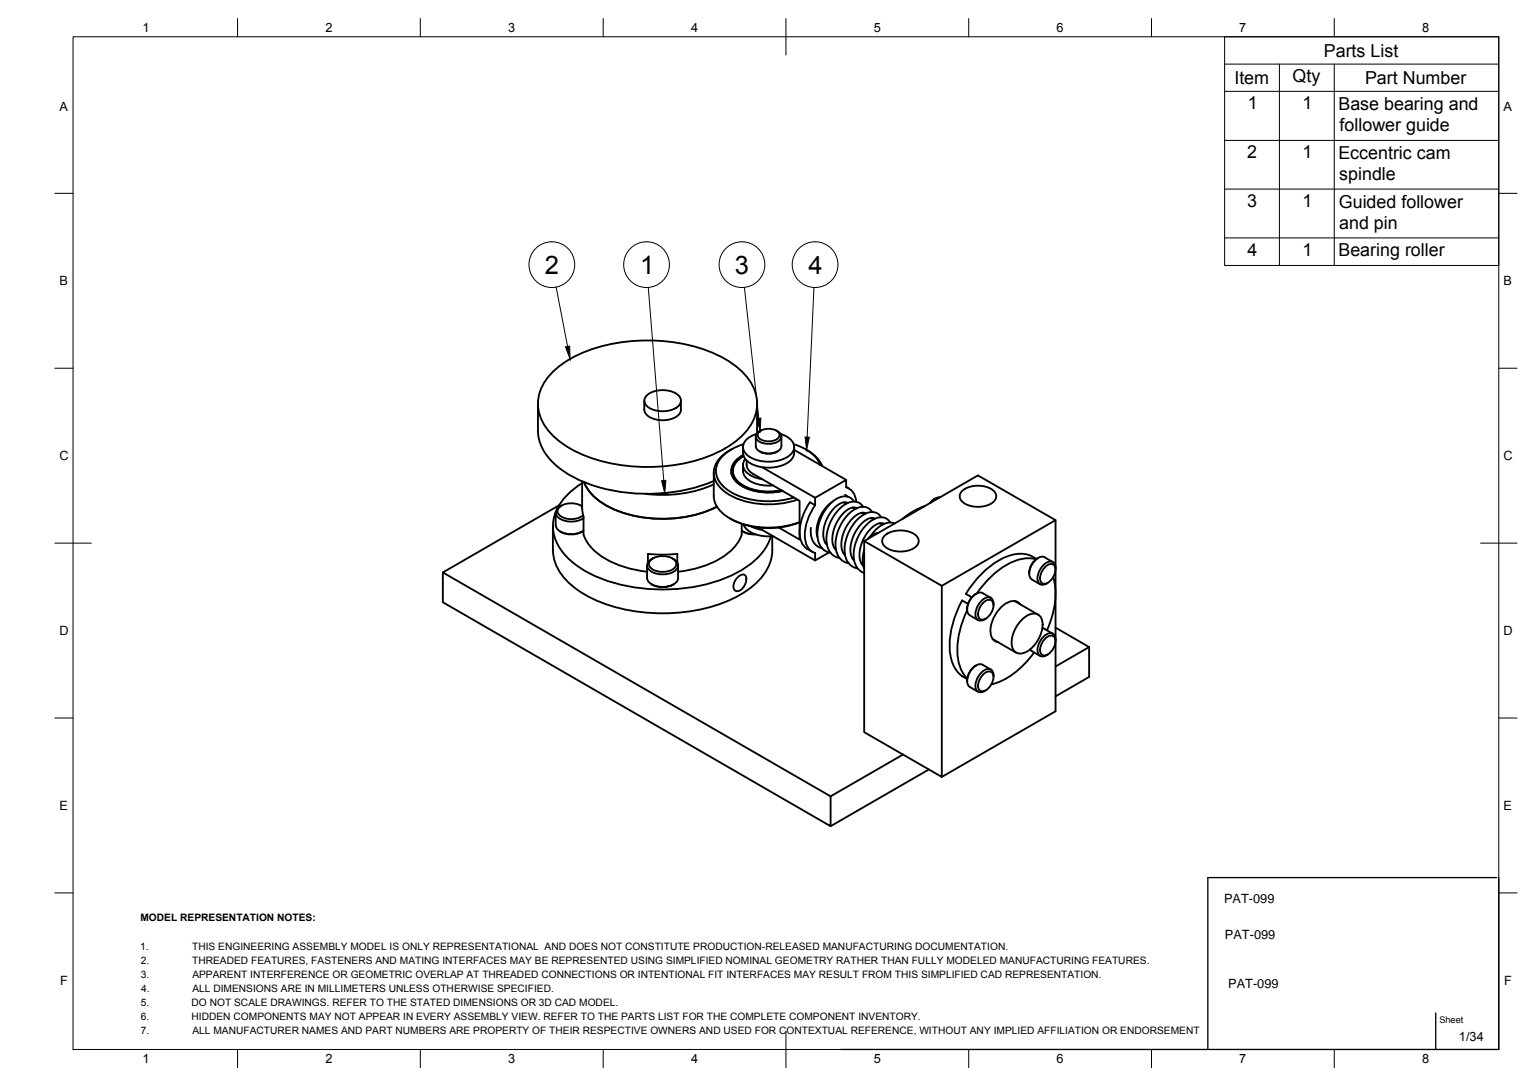
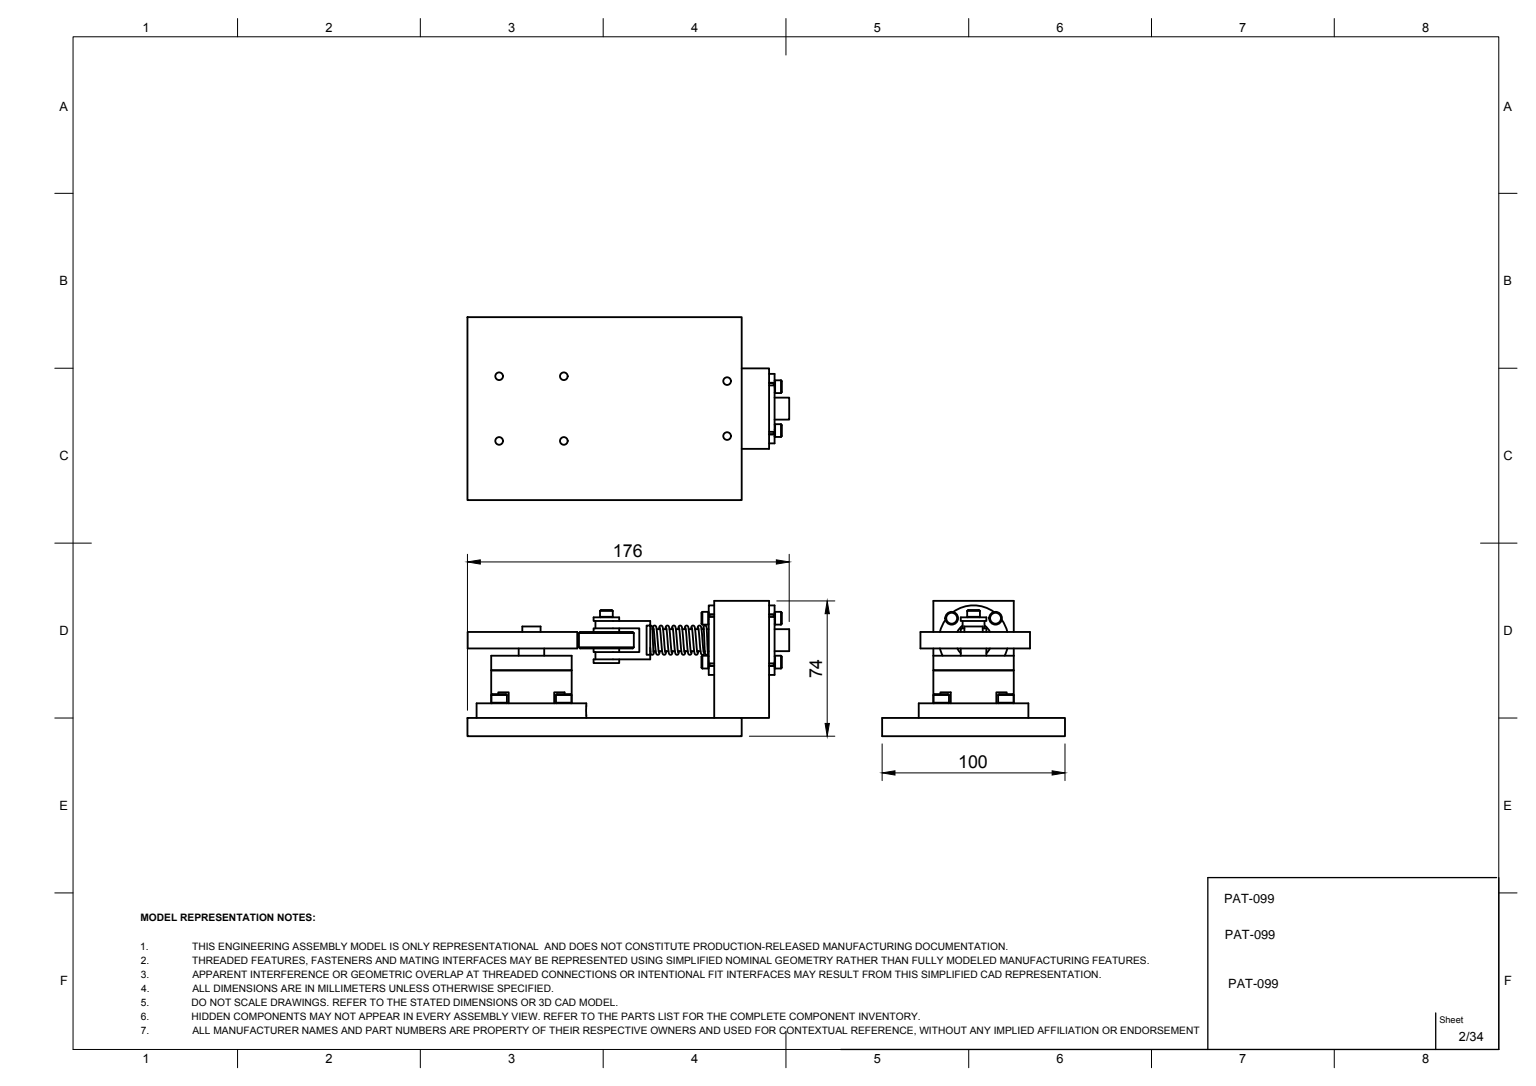
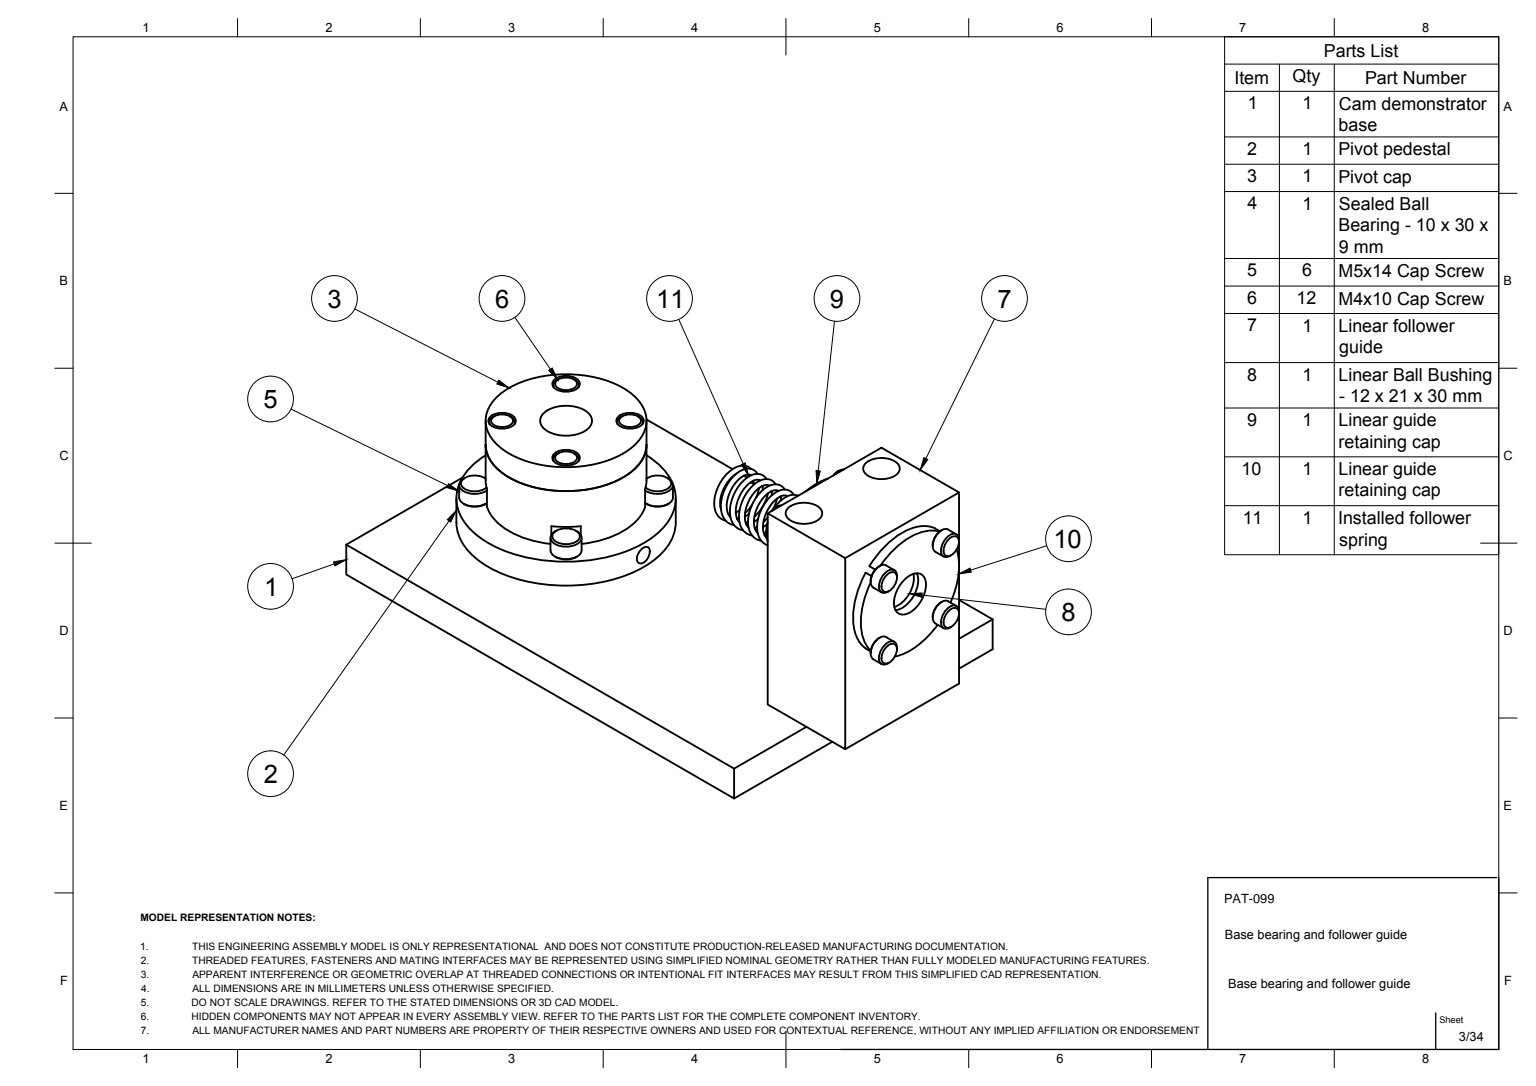
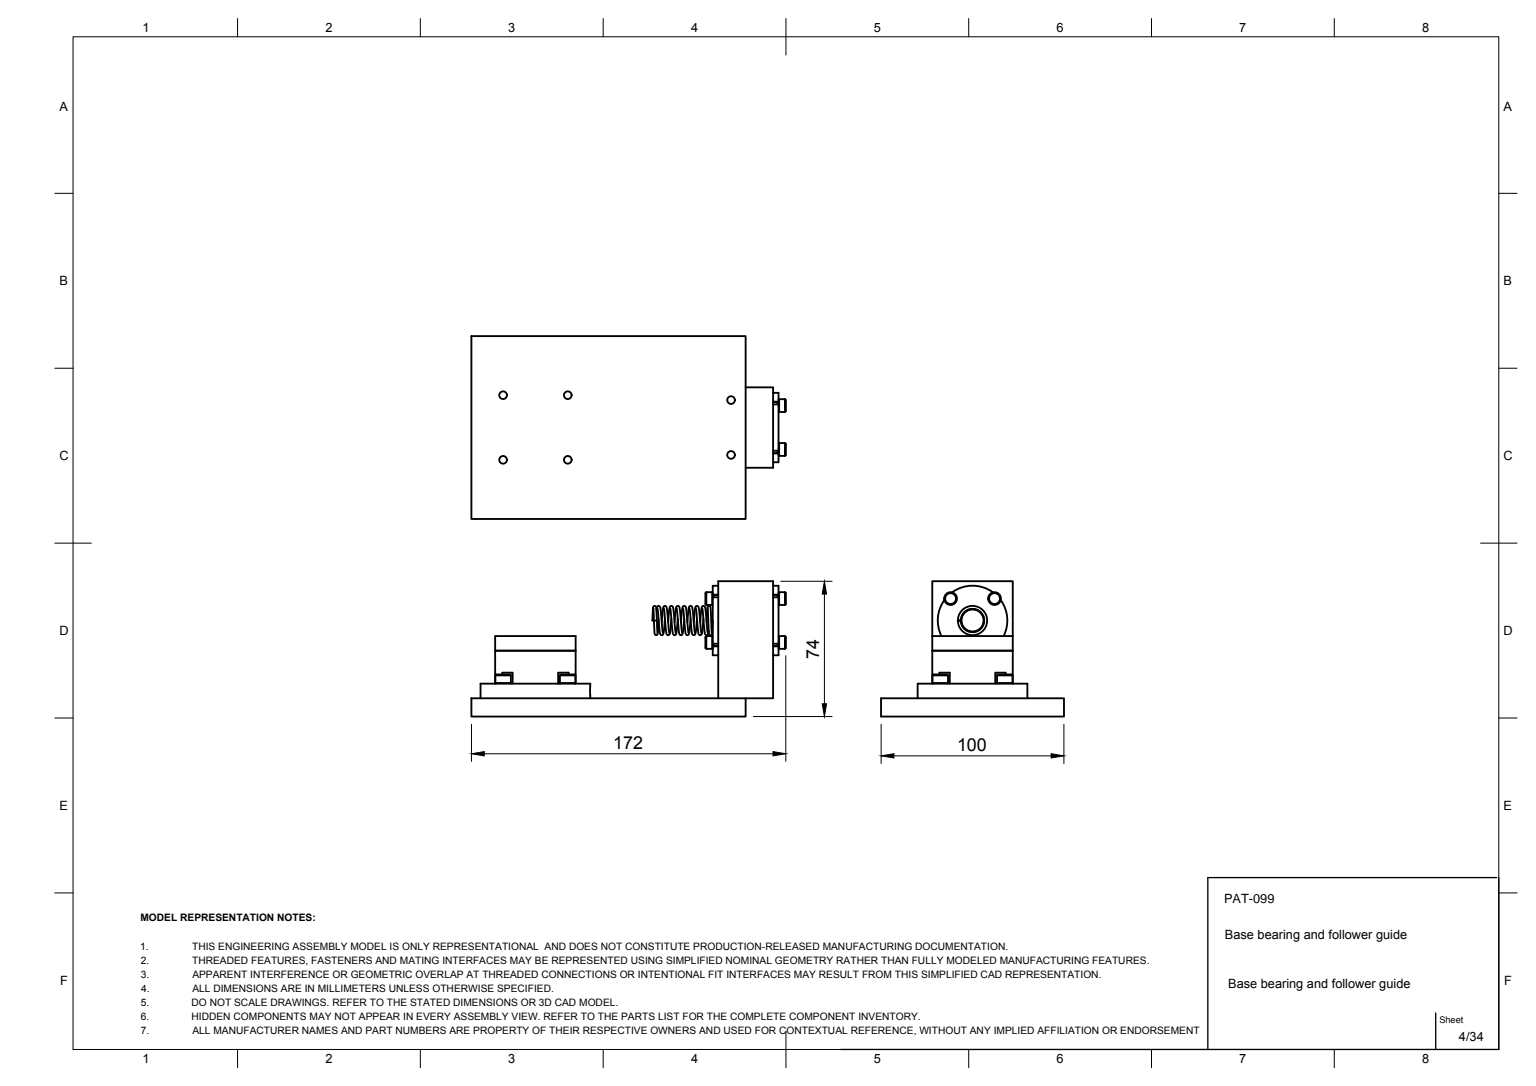
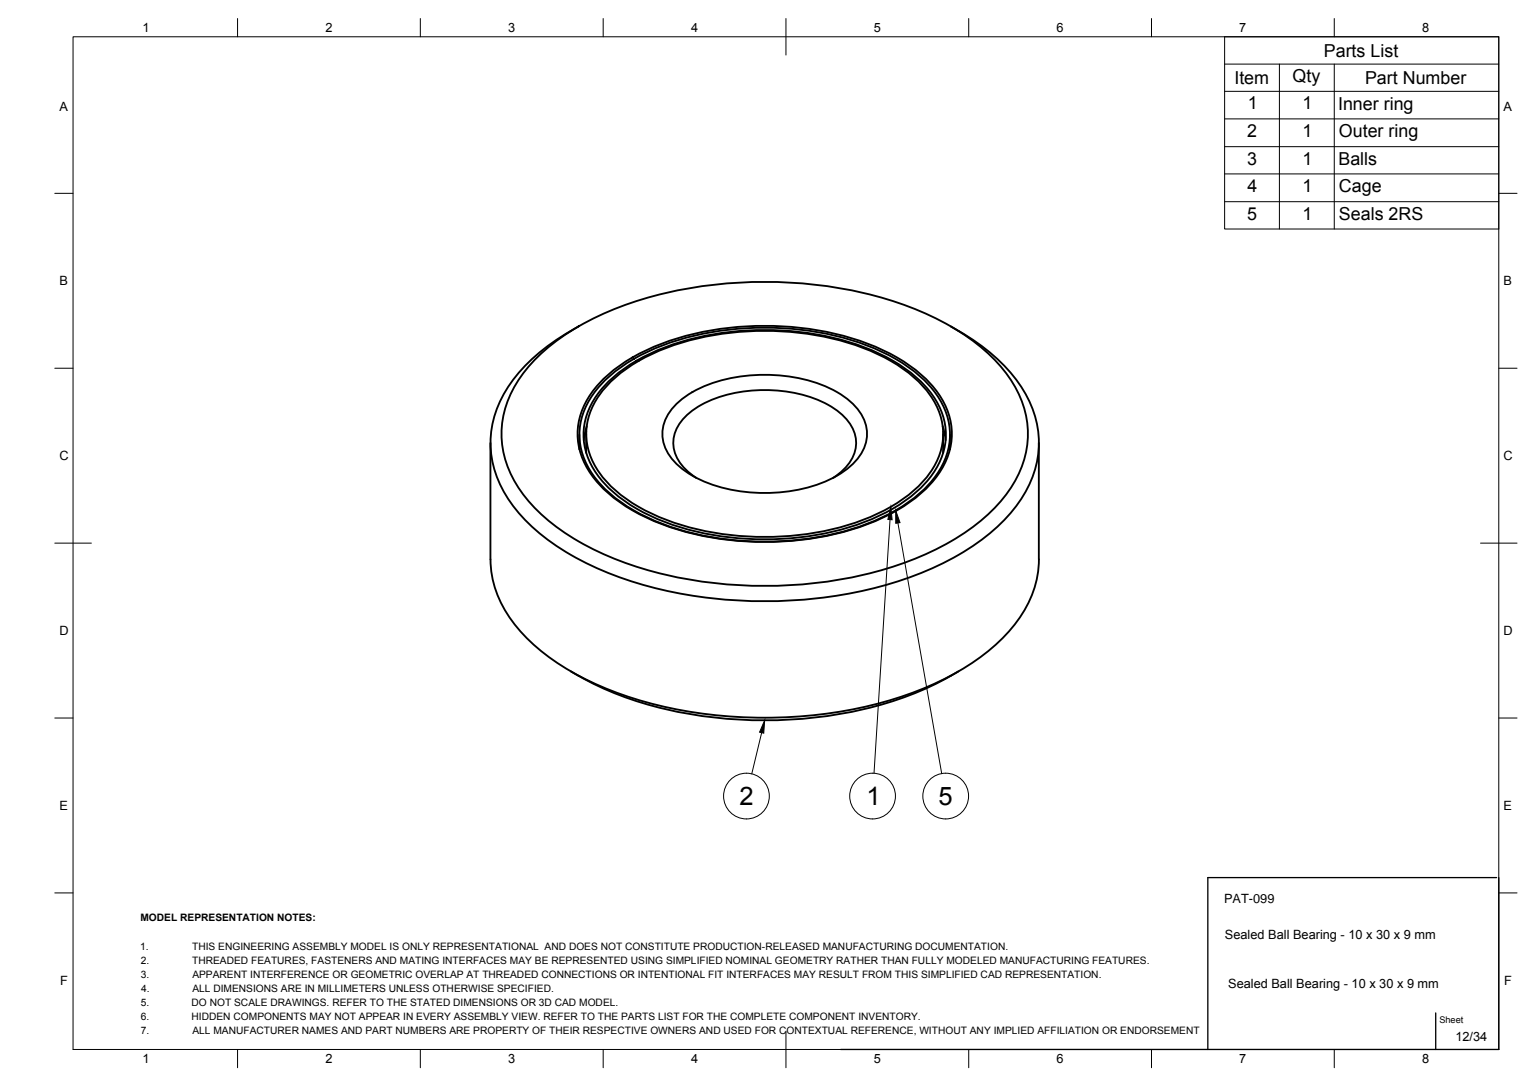
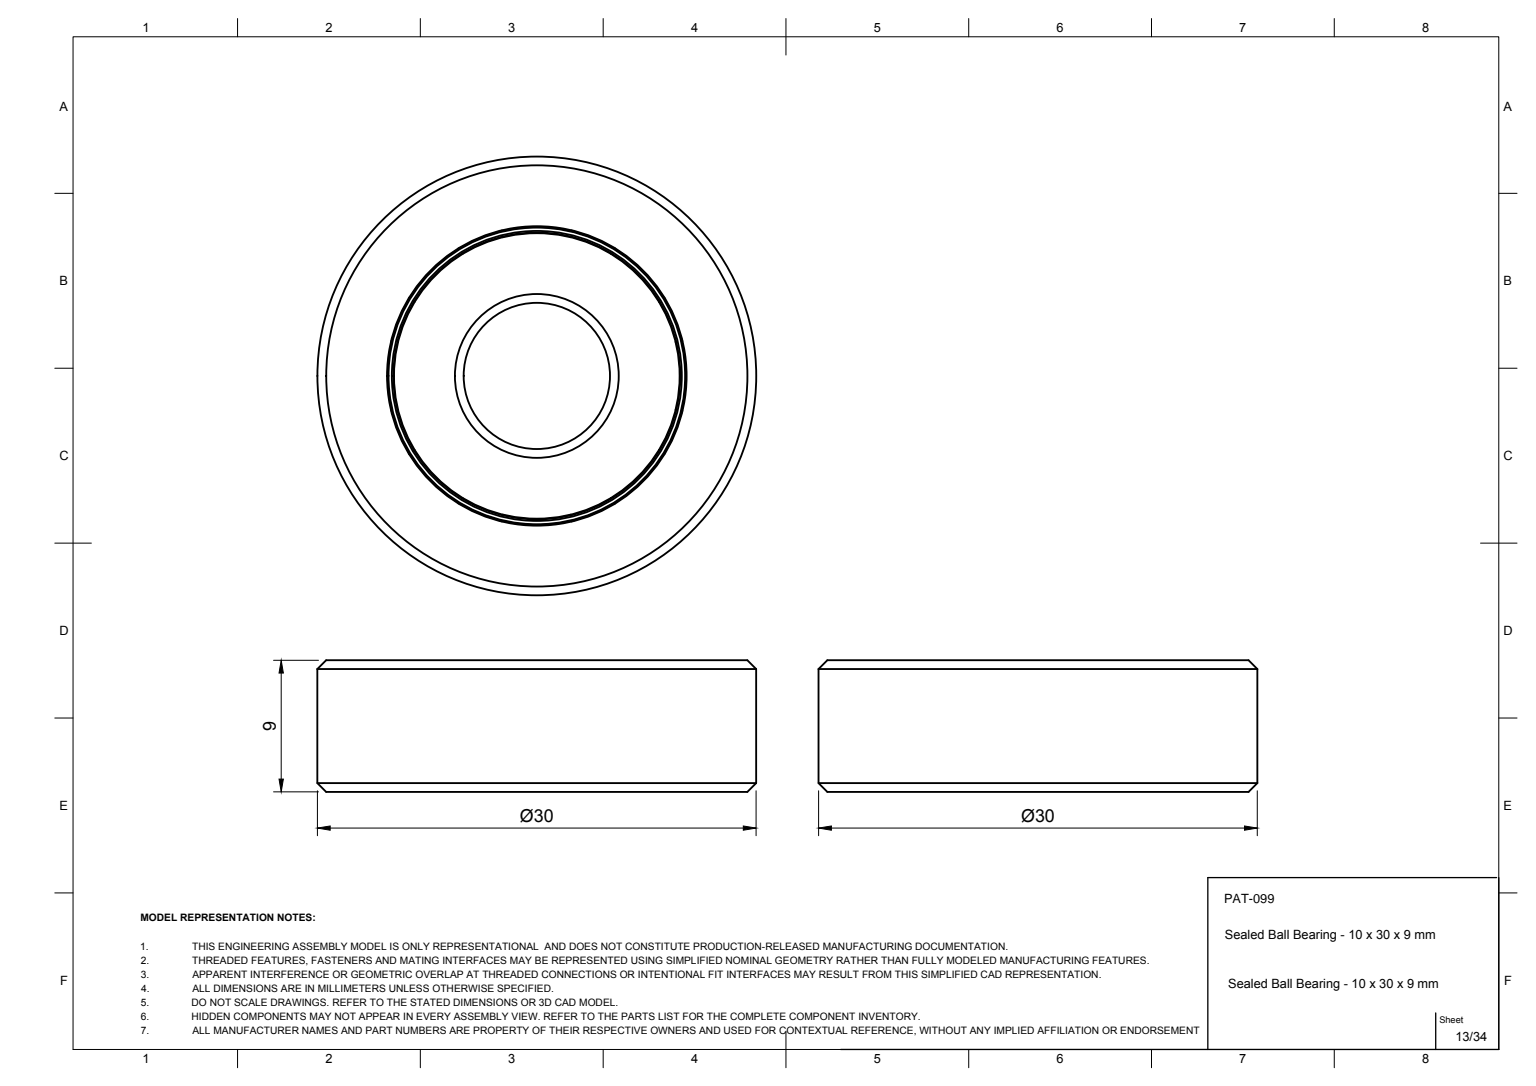
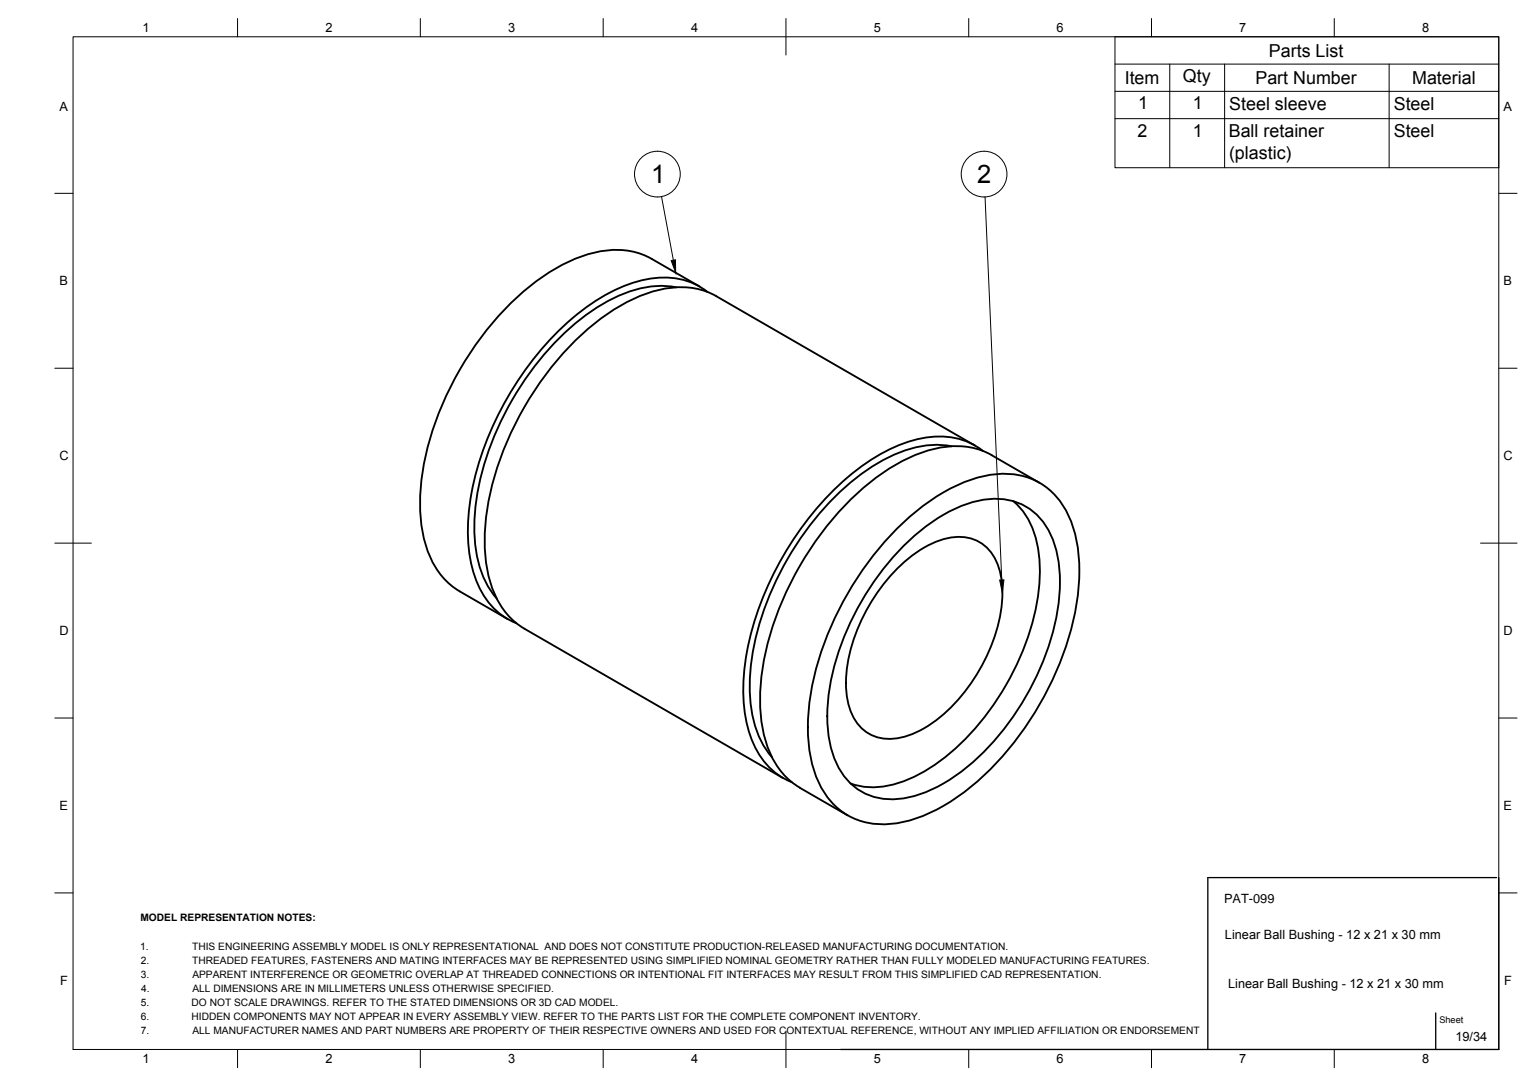
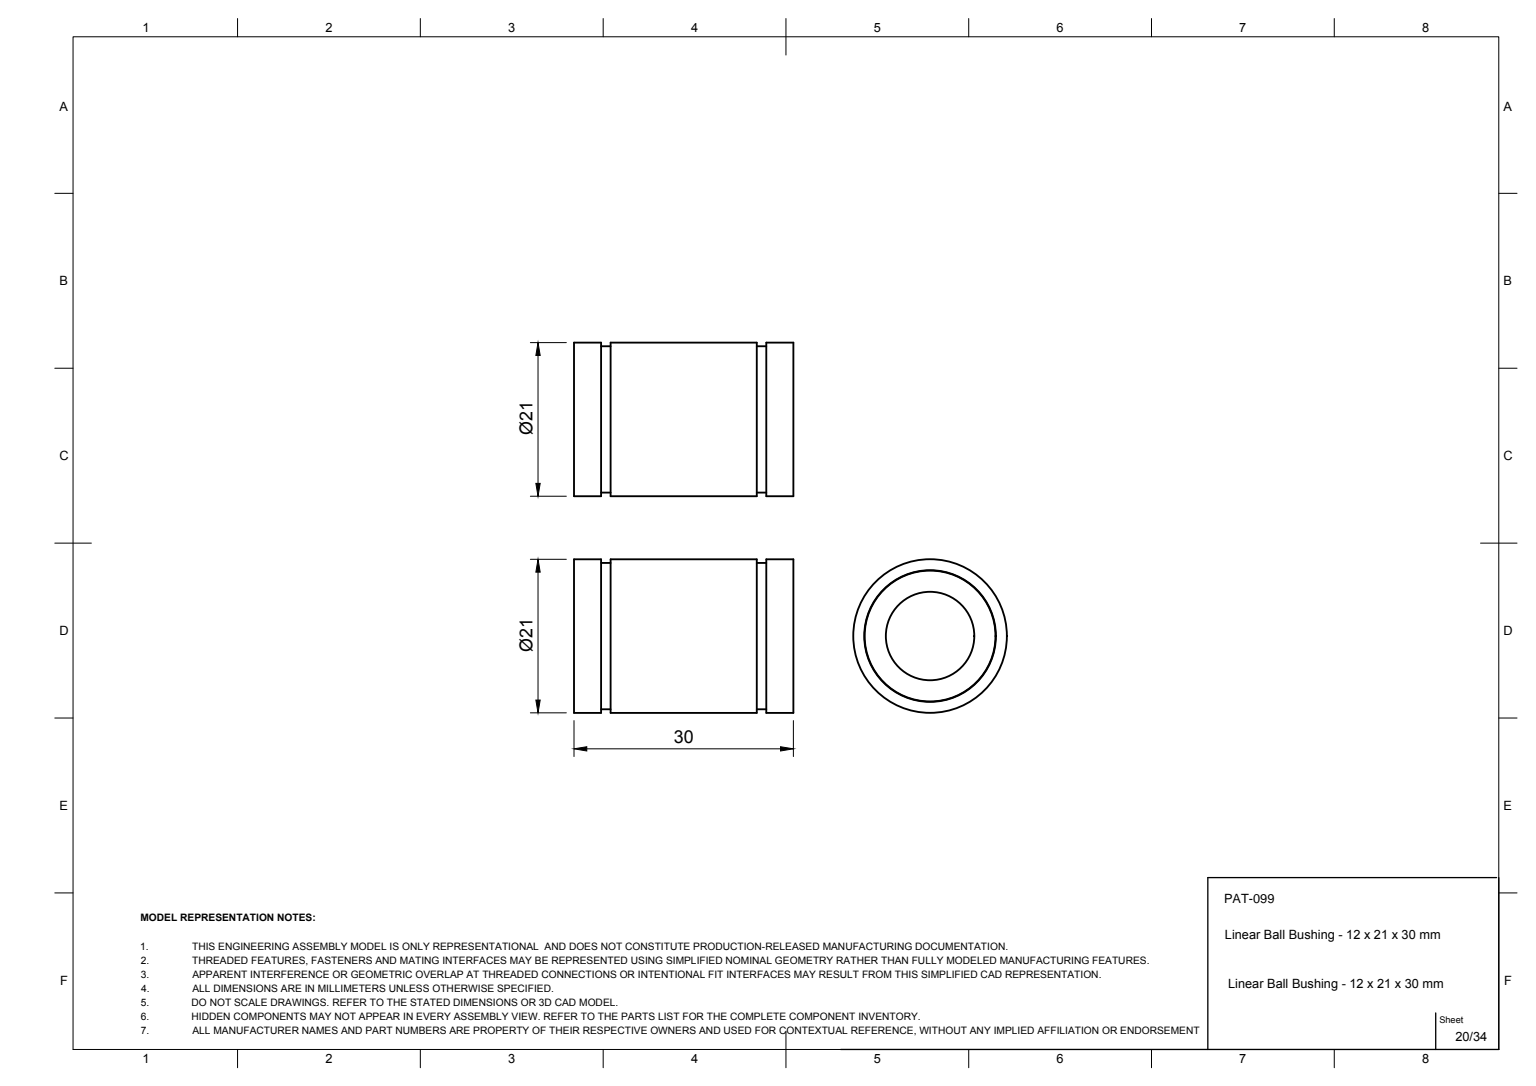
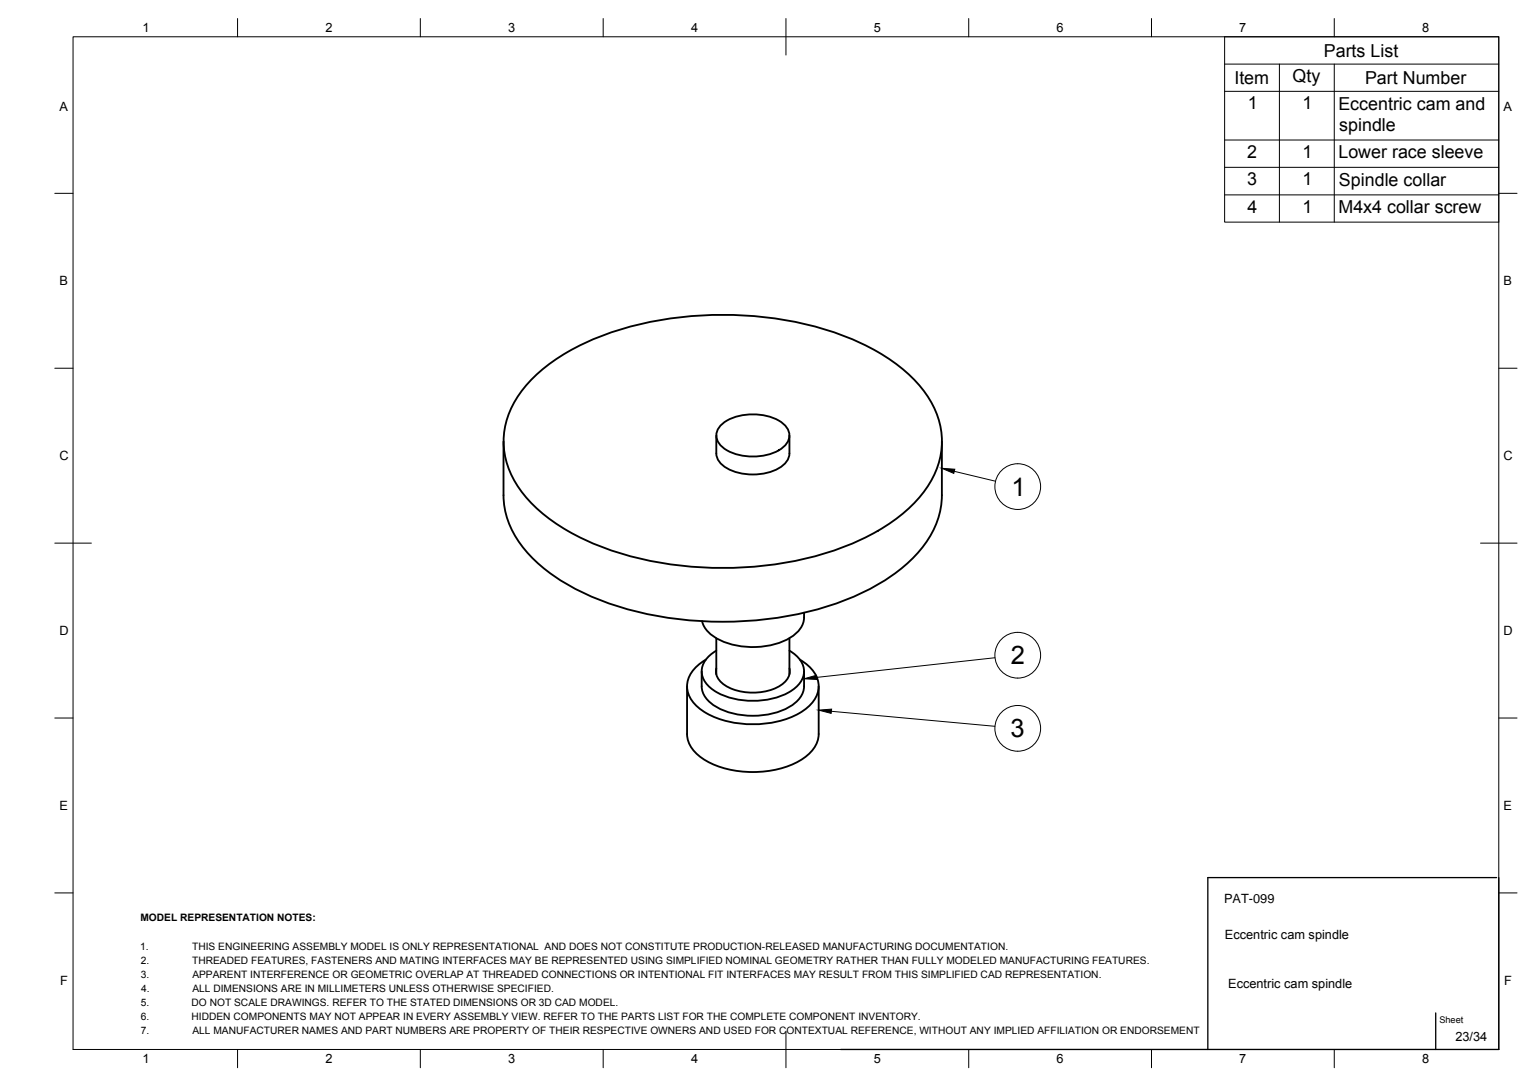
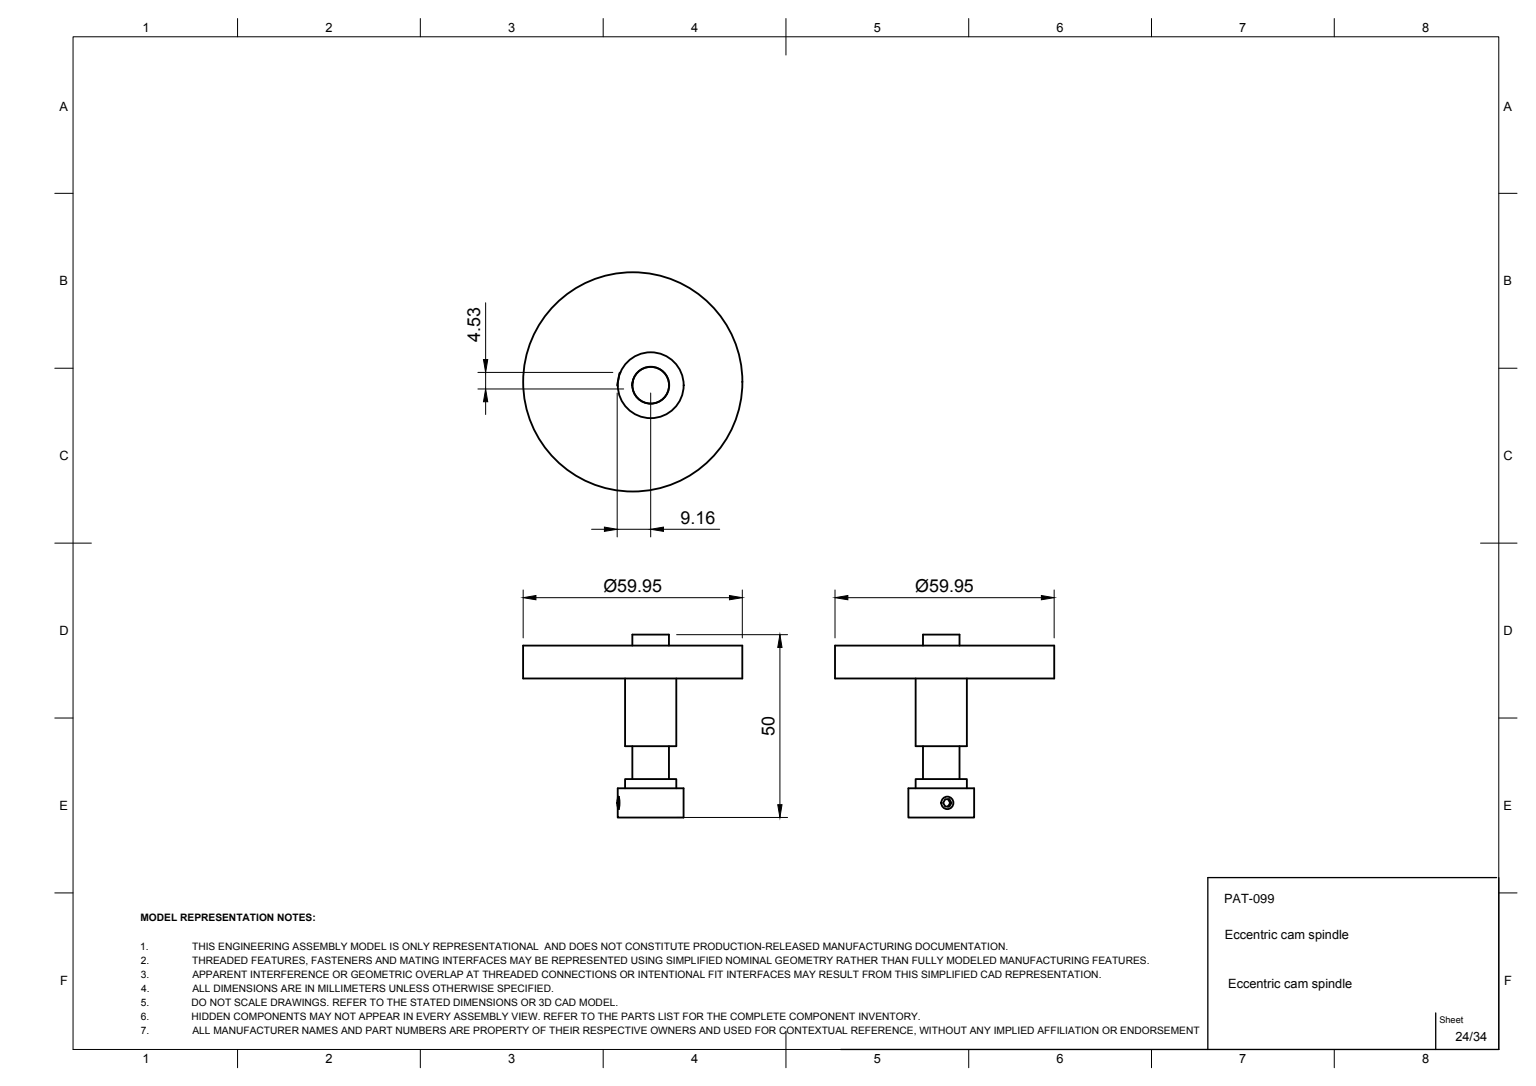
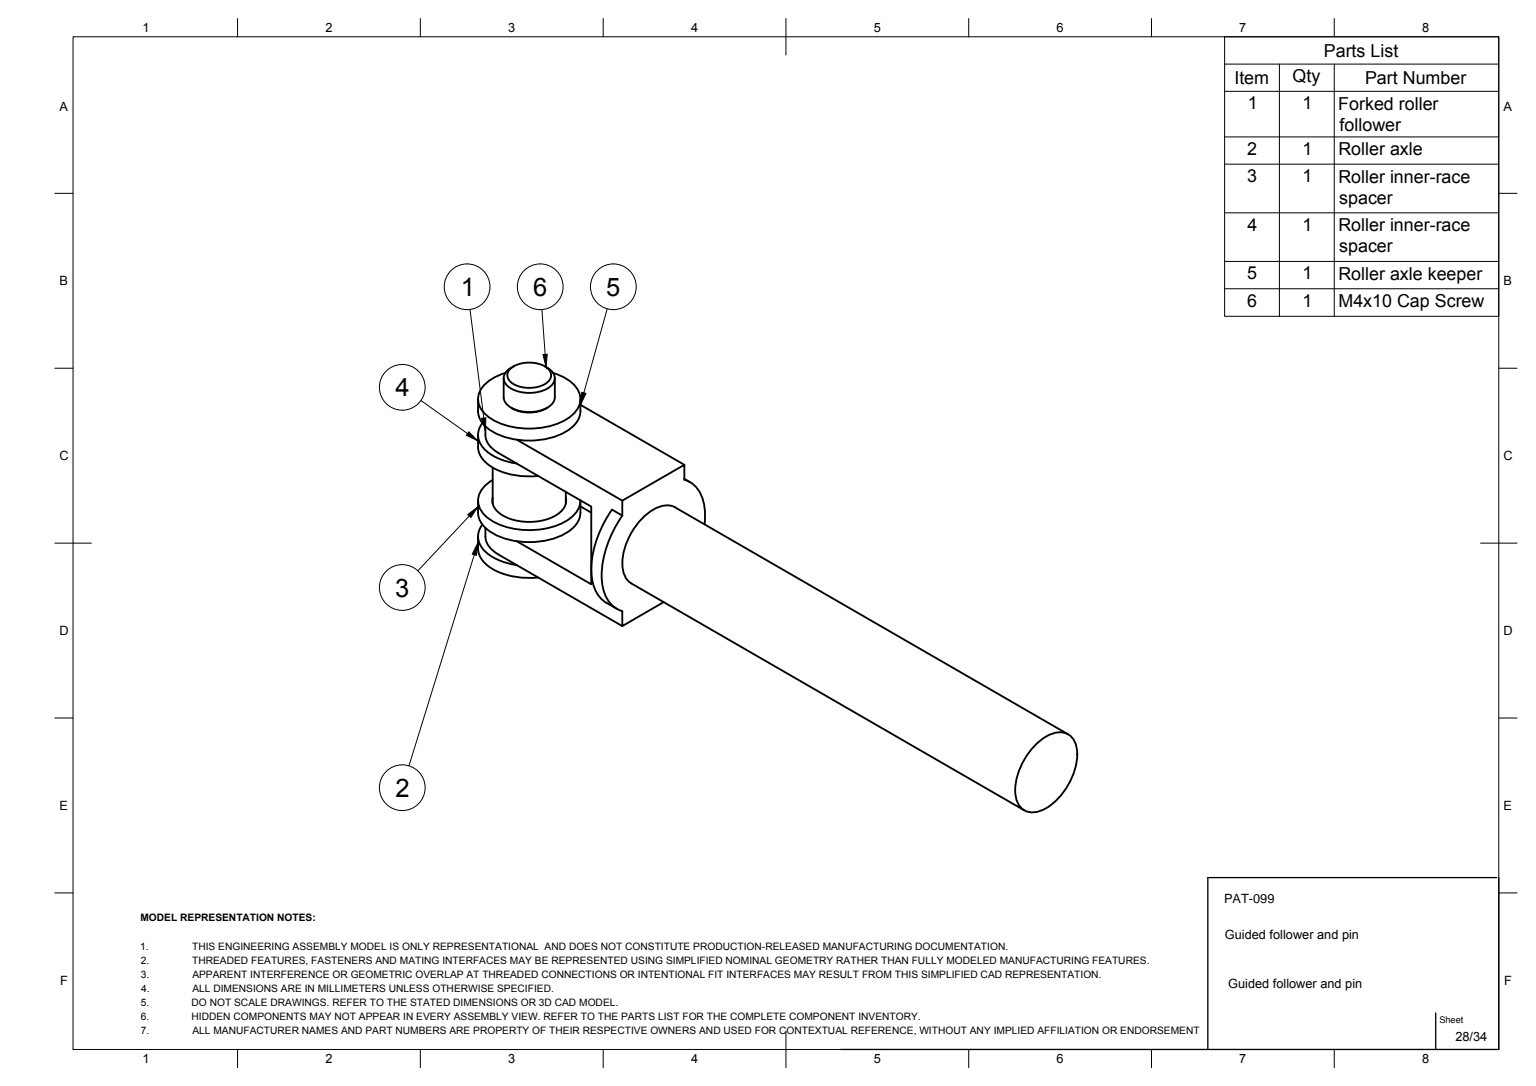
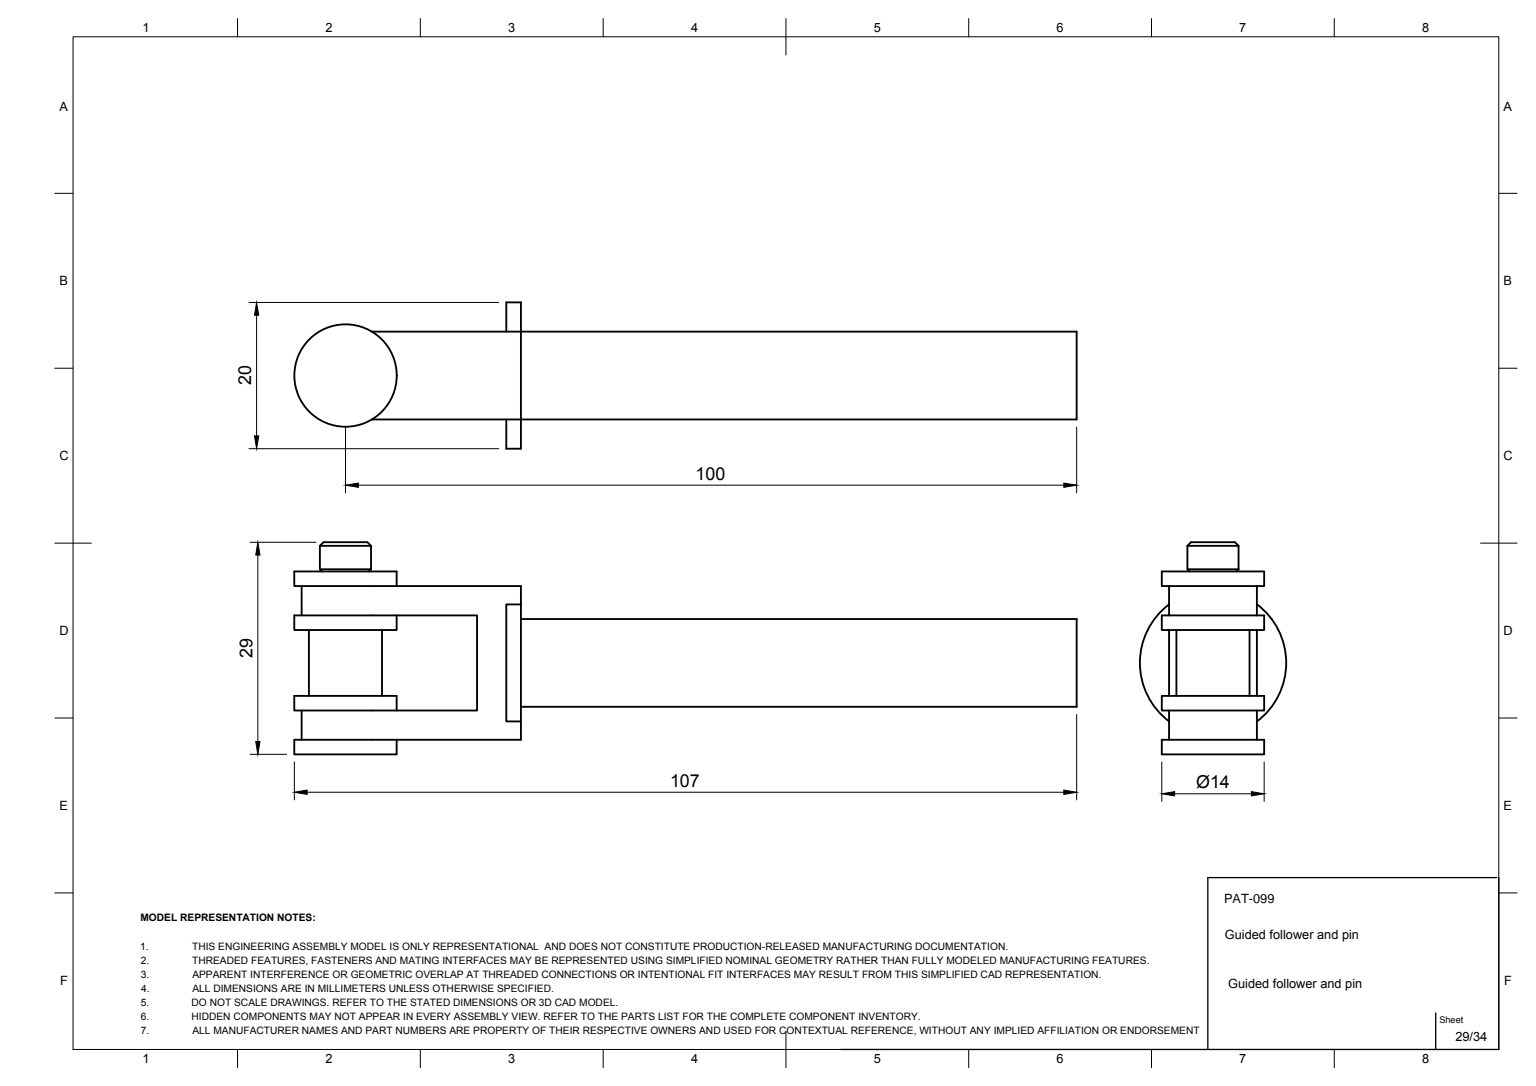
ISO-10303-21;
HEADER;
/* Generated by software containing ST-Developer
 * from STEP Tools, Inc. (www.steptools.com) 
 */

FILE_DESCRIPTION(
/* description */ ('PAT-099'),
/* implementation_level */ '2;1');

FILE_NAME(
/* name */ 'PAT-099',
/* time_stamp */ '2026-10-29T17:25:42-07:00',
/* author */ (''),
/* organization */ (''),
/* preprocessor_version */ 'ST-DEVELOPER v20.2',
/* originating_system */ 'Autodesk Translation Framework v15.17.0.0',
/* authorisation */ '');

FILE_SCHEMA (('AUTOMOTIVE_DESIGN { 1 0 10303 214 3 1 1 }'));
ENDSEC;

DATA;
#10=MECHANICAL_DESIGN_GEOMETRIC_PRESENTATION_REPRESENTATION('',(#337,#338,
#339,#340,#341,#342,#343,#344,#345,#346,#347,#348,#349,#350,#351,#352,#353,
#354,#355,#356,#357,#358,#359,#360,#361,#362,#363,#364,#365,#366,#367,#368,
#369),#11035);
#11=SPHERICAL_SURFACE('',#5544,0.23815);
#12=SPHERICAL_SURFACE('',#5546,0.23815);
#13=SPHERICAL_SURFACE('',#5548,0.23815);
#14=SPHERICAL_SURFACE('',#5550,0.23815);
#15=SPHERICAL_SURFACE('',#5552,0.23815);
#16=SPHERICAL_SURFACE('',#5554,0.23815);
#17=SPHERICAL_SURFACE('',#5556,0.23815);
#18=SPHERICAL_SURFACE('',#5558,0.23815);
#19=SPHERICAL_SURFACE('',#5561,0.247676);
#20=SPHERICAL_SURFACE('',#5577,0.247676);
#21=SPHERICAL_SURFACE('',#5582,0.247676);
#22=SPHERICAL_SURFACE('',#5587,0.247676);
#23=SPHERICAL_SURFACE('',#5592,0.247676);
#24=SPHERICAL_SURFACE('',#5597,0.247676);
#25=SPHERICAL_SURFACE('',#5602,0.247676);
#26=SPHERICAL_SURFACE('',#5610,0.247676);
#27=TOROIDAL_SURFACE('',#5504,1.,0.247676);
#28=TOROIDAL_SURFACE('',#5524,1.,0.247676);
#29=CONICAL_SURFACE('',#5324,0.4,0.785398163397448);
#30=CONICAL_SURFACE('',#5328,0.41,0.785398163397448);
#31=CONICAL_SURFACE('',#5332,0.26,0.463647609000806);
#32=CONICAL_SURFACE('',#5389,0.185,0.785398163397449);
#33=CONICAL_SURFACE('',#5484,0.325,0.785398163397448);
#34=CONICAL_SURFACE('',#5488,0.335,0.785398163397448);
#35=CONICAL_SURFACE('',#5492,0.21,0.463647609000806);
#36=CONICAL_SURFACE('',#5515,0.53,0.785398163397448);
#37=CONICAL_SURFACE('',#5522,0.53,0.785398163397448);
#38=CONICAL_SURFACE('',#5535,1.47,0.785398163397449);
#39=CONICAL_SURFACE('',#5539,1.47,0.785398163397449);
#40=ORIENTED_CLOSED_SHELL('',*,#4714,.F.);
#41=ORIENTED_CLOSED_SHELL('',*,#4725,.F.);
#42=BREP_WITH_VOIDS('Body1',#4715,(#40));
#43=BREP_WITH_VOIDS('Body1',#4726,(#41));
#44=ITEM_DEFINED_TRANSFORMATION($,$,#5260,#5309);
#45=ITEM_DEFINED_TRANSFORMATION($,$,#5292,#5310);
#46=ITEM_DEFINED_TRANSFORMATION($,$,#5336,#5392);
#47=ITEM_DEFINED_TRANSFORMATION($,$,#5354,#5393);
#48=ITEM_DEFINED_TRANSFORMATION($,$,#5363,#5394);
#49=ITEM_DEFINED_TRANSFORMATION($,$,#5377,#5395);
#50=ITEM_DEFINED_TRANSFORMATION($,$,#5397,#5495);
#51=ITEM_DEFINED_TRANSFORMATION($,$,#5430,#5496);
#52=ITEM_DEFINED_TRANSFORMATION($,$,#5444,#5497);
#53=ITEM_DEFINED_TRANSFORMATION($,$,#5453,#5498);
#54=ITEM_DEFINED_TRANSFORMATION($,$,#5462,#5499);
#55=ITEM_DEFINED_TRANSFORMATION($,$,#5471,#5500);
#56=ITEM_DEFINED_TRANSFORMATION($,$,#5503,#5631);
#57=ITEM_DEFINED_TRANSFORMATION($,$,#5523,#5632);
#58=ITEM_DEFINED_TRANSFORMATION($,$,#5543,#5633);
#59=ITEM_DEFINED_TRANSFORMATION($,$,#5560,#5634);
#60=ITEM_DEFINED_TRANSFORMATION($,$,#5614,#5635);
#61=ITEM_DEFINED_TRANSFORMATION($,$,#5018,#5636);
#62=ITEM_DEFINED_TRANSFORMATION($,$,#5043,#5637);
#63=ITEM_DEFINED_TRANSFORMATION($,$,#5083,#5638);
#64=ITEM_DEFINED_TRANSFORMATION($,$,#5113,#5639);
#65=ITEM_DEFINED_TRANSFORMATION($,$,#5143,#5640);
#66=ITEM_DEFINED_TRANSFORMATION($,$,#5148,#5641);
#67=ITEM_DEFINED_TRANSFORMATION($,$,#5218,#5642);
#68=ITEM_DEFINED_TRANSFORMATION($,$,#5502,#5643);
#69=ITEM_DEFINED_TRANSFORMATION($,$,#5311,#5644);
#70=ITEM_DEFINED_TRANSFORMATION($,$,#5471,#5645);
#71=ITEM_DEFINED_TRANSFORMATION($,$,#5311,#5646);
#72=ITEM_DEFINED_TRANSFORMATION($,$,#5471,#5647);
#73=ITEM_DEFINED_TRANSFORMATION($,$,#5311,#5648);
#74=ITEM_DEFINED_TRANSFORMATION($,$,#5471,#5649);
#75=ITEM_DEFINED_TRANSFORMATION($,$,#5311,#5650);
#76=ITEM_DEFINED_TRANSFORMATION($,$,#5471,#5651);
#77=ITEM_DEFINED_TRANSFORMATION($,$,#5259,#5652);
#78=ITEM_DEFINED_TRANSFORMATION($,$,#5311,#5653);
#79=ITEM_DEFINED_TRANSFORMATION($,$,#5311,#5654);
#80=ITEM_DEFINED_TRANSFORMATION($,$,#5471,#5655);
#81=ITEM_DEFINED_TRANSFORMATION($,$,#5471,#5656);
#82=ITEM_DEFINED_TRANSFORMATION($,$,#5471,#5657);
#83=ITEM_DEFINED_TRANSFORMATION($,$,#5471,#5658);
#84=ITEM_DEFINED_TRANSFORMATION($,$,#5471,#5659);
#85=ITEM_DEFINED_TRANSFORMATION($,$,#5471,#5660);
#86=ITEM_DEFINED_TRANSFORMATION($,$,#5471,#5661);
#87=ITEM_DEFINED_TRANSFORMATION($,$,#5471,#5662);
#88=ITEM_DEFINED_TRANSFORMATION($,$,#5502,#5663);
#89=ITEM_DEFINED_TRANSFORMATION($,$,#5017,#5664);
#90=ITEM_DEFINED_TRANSFORMATION($,$,#5335,#5665);
#91=ITEM_DEFINED_TRANSFORMATION($,$,#5396,#5666);
#92=ITEM_DEFINED_TRANSFORMATION($,$,#5501,#5667);
#93=(
REPRESENTATION_RELATIONSHIP($,$,#11163,#11162)
REPRESENTATION_RELATIONSHIP_WITH_TRANSFORMATION(#44)
SHAPE_REPRESENTATION_RELATIONSHIP()
);
#94=(
REPRESENTATION_RELATIONSHIP($,$,#11164,#11162)
REPRESENTATION_RELATIONSHIP_WITH_TRANSFORMATION(#45)
SHAPE_REPRESENTATION_RELATIONSHIP()
);
#95=(
REPRESENTATION_RELATIONSHIP($,$,#11167,#11166)
REPRESENTATION_RELATIONSHIP_WITH_TRANSFORMATION(#46)
SHAPE_REPRESENTATION_RELATIONSHIP()
);
#96=(
REPRESENTATION_RELATIONSHIP($,$,#11168,#11166)
REPRESENTATION_RELATIONSHIP_WITH_TRANSFORMATION(#47)
SHAPE_REPRESENTATION_RELATIONSHIP()
);
#97=(
REPRESENTATION_RELATIONSHIP($,$,#11169,#11166)
REPRESENTATION_RELATIONSHIP_WITH_TRANSFORMATION(#48)
SHAPE_REPRESENTATION_RELATIONSHIP()
);
#98=(
REPRESENTATION_RELATIONSHIP($,$,#11170,#11166)
REPRESENTATION_RELATIONSHIP_WITH_TRANSFORMATION(#49)
SHAPE_REPRESENTATION_RELATIONSHIP()
);
#99=(
REPRESENTATION_RELATIONSHIP($,$,#11172,#11171)
REPRESENTATION_RELATIONSHIP_WITH_TRANSFORMATION(#50)
SHAPE_REPRESENTATION_RELATIONSHIP()
);
#100=(
REPRESENTATION_RELATIONSHIP($,$,#11173,#11171)
REPRESENTATION_RELATIONSHIP_WITH_TRANSFORMATION(#51)
SHAPE_REPRESENTATION_RELATIONSHIP()
);
#101=(
REPRESENTATION_RELATIONSHIP($,$,#11174,#11171)
REPRESENTATION_RELATIONSHIP_WITH_TRANSFORMATION(#52)
SHAPE_REPRESENTATION_RELATIONSHIP()
);
#102=(
REPRESENTATION_RELATIONSHIP($,$,#11175,#11171)
REPRESENTATION_RELATIONSHIP_WITH_TRANSFORMATION(#53)
SHAPE_REPRESENTATION_RELATIONSHIP()
);
#103=(
REPRESENTATION_RELATIONSHIP($,$,#11176,#11171)
REPRESENTATION_RELATIONSHIP_WITH_TRANSFORMATION(#54)
SHAPE_REPRESENTATION_RELATIONSHIP()
);
#104=(
REPRESENTATION_RELATIONSHIP($,$,#11177,#11171)
REPRESENTATION_RELATIONSHIP_WITH_TRANSFORMATION(#55)
SHAPE_REPRESENTATION_RELATIONSHIP()
);
#105=(
REPRESENTATION_RELATIONSHIP($,$,#11180,#11179)
REPRESENTATION_RELATIONSHIP_WITH_TRANSFORMATION(#56)
SHAPE_REPRESENTATION_RELATIONSHIP()
);
#106=(
REPRESENTATION_RELATIONSHIP($,$,#11181,#11179)
REPRESENTATION_RELATIONSHIP_WITH_TRANSFORMATION(#57)
SHAPE_REPRESENTATION_RELATIONSHIP()
);
#107=(
REPRESENTATION_RELATIONSHIP($,$,#11182,#11179)
REPRESENTATION_RELATIONSHIP_WITH_TRANSFORMATION(#58)
SHAPE_REPRESENTATION_RELATIONSHIP()
);
#108=(
REPRESENTATION_RELATIONSHIP($,$,#11183,#11179)
REPRESENTATION_RELATIONSHIP_WITH_TRANSFORMATION(#59)
SHAPE_REPRESENTATION_RELATIONSHIP()
);
#109=(
REPRESENTATION_RELATIONSHIP($,$,#11184,#11179)
REPRESENTATION_RELATIONSHIP_WITH_TRANSFORMATION(#60)
SHAPE_REPRESENTATION_RELATIONSHIP()
);
#110=(
REPRESENTATION_RELATIONSHIP($,$,#11155,#11154)
REPRESENTATION_RELATIONSHIP_WITH_TRANSFORMATION(#61)
SHAPE_REPRESENTATION_RELATIONSHIP()
);
#111=(
REPRESENTATION_RELATIONSHIP($,$,#11156,#11154)
REPRESENTATION_RELATIONSHIP_WITH_TRANSFORMATION(#62)
SHAPE_REPRESENTATION_RELATIONSHIP()
);
#112=(
REPRESENTATION_RELATIONSHIP($,$,#11157,#11154)
REPRESENTATION_RELATIONSHIP_WITH_TRANSFORMATION(#63)
SHAPE_REPRESENTATION_RELATIONSHIP()
);
#113=(
REPRESENTATION_RELATIONSHIP($,$,#11158,#11154)
REPRESENTATION_RELATIONSHIP_WITH_TRANSFORMATION(#64)
SHAPE_REPRESENTATION_RELATIONSHIP()
);
#114=(
REPRESENTATION_RELATIONSHIP($,$,#11159,#11154)
REPRESENTATION_RELATIONSHIP_WITH_TRANSFORMATION(#65)
SHAPE_REPRESENTATION_RELATIONSHIP()
);
#115=(
REPRESENTATION_RELATIONSHIP($,$,#11160,#11154)
REPRESENTATION_RELATIONSHIP_WITH_TRANSFORMATION(#66)
SHAPE_REPRESENTATION_RELATIONSHIP()
);
#116=(
REPRESENTATION_RELATIONSHIP($,$,#11161,#11154)
REPRESENTATION_RELATIONSHIP_WITH_TRANSFORMATION(#67)
SHAPE_REPRESENTATION_RELATIONSHIP()
);
#117=(
REPRESENTATION_RELATIONSHIP($,$,#11179,#11154)
REPRESENTATION_RELATIONSHIP_WITH_TRANSFORMATION(#68)
SHAPE_REPRESENTATION_RELATIONSHIP()
);
#118=(
REPRESENTATION_RELATIONSHIP($,$,#11165,#11154)
REPRESENTATION_RELATIONSHIP_WITH_TRANSFORMATION(#69)
SHAPE_REPRESENTATION_RELATIONSHIP()
);
#119=(
REPRESENTATION_RELATIONSHIP($,$,#11177,#11154)
REPRESENTATION_RELATIONSHIP_WITH_TRANSFORMATION(#70)
SHAPE_REPRESENTATION_RELATIONSHIP()
);
#120=(
REPRESENTATION_RELATIONSHIP($,$,#11165,#11154)
REPRESENTATION_RELATIONSHIP_WITH_TRANSFORMATION(#71)
SHAPE_REPRESENTATION_RELATIONSHIP()
);
#121=(
REPRESENTATION_RELATIONSHIP($,$,#11177,#11154)
REPRESENTATION_RELATIONSHIP_WITH_TRANSFORMATION(#72)
SHAPE_REPRESENTATION_RELATIONSHIP()
);
#122=(
REPRESENTATION_RELATIONSHIP($,$,#11165,#11154)
REPRESENTATION_RELATIONSHIP_WITH_TRANSFORMATION(#73)
SHAPE_REPRESENTATION_RELATIONSHIP()
);
#123=(
REPRESENTATION_RELATIONSHIP($,$,#11177,#11154)
REPRESENTATION_RELATIONSHIP_WITH_TRANSFORMATION(#74)
SHAPE_REPRESENTATION_RELATIONSHIP()
);
#124=(
REPRESENTATION_RELATIONSHIP($,$,#11165,#11154)
REPRESENTATION_RELATIONSHIP_WITH_TRANSFORMATION(#75)
SHAPE_REPRESENTATION_RELATIONSHIP()
);
#125=(
REPRESENTATION_RELATIONSHIP($,$,#11177,#11154)
REPRESENTATION_RELATIONSHIP_WITH_TRANSFORMATION(#76)
SHAPE_REPRESENTATION_RELATIONSHIP()
);
#126=(
REPRESENTATION_RELATIONSHIP($,$,#11162,#11154)
REPRESENTATION_RELATIONSHIP_WITH_TRANSFORMATION(#77)
SHAPE_REPRESENTATION_RELATIONSHIP()
);
#127=(
REPRESENTATION_RELATIONSHIP($,$,#11165,#11154)
REPRESENTATION_RELATIONSHIP_WITH_TRANSFORMATION(#78)
SHAPE_REPRESENTATION_RELATIONSHIP()
);
#128=(
REPRESENTATION_RELATIONSHIP($,$,#11165,#11154)
REPRESENTATION_RELATIONSHIP_WITH_TRANSFORMATION(#79)
SHAPE_REPRESENTATION_RELATIONSHIP()
);
#129=(
REPRESENTATION_RELATIONSHIP($,$,#11177,#11154)
REPRESENTATION_RELATIONSHIP_WITH_TRANSFORMATION(#80)
SHAPE_REPRESENTATION_RELATIONSHIP()
);
#130=(
REPRESENTATION_RELATIONSHIP($,$,#11177,#11154)
REPRESENTATION_RELATIONSHIP_WITH_TRANSFORMATION(#81)
SHAPE_REPRESENTATION_RELATIONSHIP()
);
#131=(
REPRESENTATION_RELATIONSHIP($,$,#11177,#11154)
REPRESENTATION_RELATIONSHIP_WITH_TRANSFORMATION(#82)
SHAPE_REPRESENTATION_RELATIONSHIP()
);
#132=(
REPRESENTATION_RELATIONSHIP($,$,#11177,#11154)
REPRESENTATION_RELATIONSHIP_WITH_TRANSFORMATION(#83)
SHAPE_REPRESENTATION_RELATIONSHIP()
);
#133=(
REPRESENTATION_RELATIONSHIP($,$,#11177,#11154)
REPRESENTATION_RELATIONSHIP_WITH_TRANSFORMATION(#84)
SHAPE_REPRESENTATION_RELATIONSHIP()
);
#134=(
REPRESENTATION_RELATIONSHIP($,$,#11177,#11154)
REPRESENTATION_RELATIONSHIP_WITH_TRANSFORMATION(#85)
SHAPE_REPRESENTATION_RELATIONSHIP()
);
#135=(
REPRESENTATION_RELATIONSHIP($,$,#11177,#11154)
REPRESENTATION_RELATIONSHIP_WITH_TRANSFORMATION(#86)
SHAPE_REPRESENTATION_RELATIONSHIP()
);
#136=(
REPRESENTATION_RELATIONSHIP($,$,#11177,#11154)
REPRESENTATION_RELATIONSHIP_WITH_TRANSFORMATION(#87)
SHAPE_REPRESENTATION_RELATIONSHIP()
);
#137=(
REPRESENTATION_RELATIONSHIP($,$,#11179,#11178)
REPRESENTATION_RELATIONSHIP_WITH_TRANSFORMATION(#88)
SHAPE_REPRESENTATION_RELATIONSHIP()
);
#138=(
REPRESENTATION_RELATIONSHIP($,$,#11154,#11153)
REPRESENTATION_RELATIONSHIP_WITH_TRANSFORMATION(#89)
SHAPE_REPRESENTATION_RELATIONSHIP()
);
#139=(
REPRESENTATION_RELATIONSHIP($,$,#11166,#11153)
REPRESENTATION_RELATIONSHIP_WITH_TRANSFORMATION(#90)
SHAPE_REPRESENTATION_RELATIONSHIP()
);
#140=(
REPRESENTATION_RELATIONSHIP($,$,#11171,#11153)
REPRESENTATION_RELATIONSHIP_WITH_TRANSFORMATION(#91)
SHAPE_REPRESENTATION_RELATIONSHIP()
);
#141=(
REPRESENTATION_RELATIONSHIP($,$,#11178,#11153)
REPRESENTATION_RELATIONSHIP_WITH_TRANSFORMATION(#92)
SHAPE_REPRESENTATION_RELATIONSHIP()
);
#142=CONTEXT_DEPENDENT_SHAPE_REPRESENTATION(#93,#11084);
#143=CONTEXT_DEPENDENT_SHAPE_REPRESENTATION(#94,#11085);
#144=CONTEXT_DEPENDENT_SHAPE_REPRESENTATION(#95,#11092);
#145=CONTEXT_DEPENDENT_SHAPE_REPRESENTATION(#96,#11093);
#146=CONTEXT_DEPENDENT_SHAPE_REPRESENTATION(#97,#11094);
#147=CONTEXT_DEPENDENT_SHAPE_REPRESENTATION(#98,#11095);
#148=CONTEXT_DEPENDENT_SHAPE_REPRESENTATION(#99,#11103);
#149=CONTEXT_DEPENDENT_SHAPE_REPRESENTATION(#100,#11104);
#150=CONTEXT_DEPENDENT_SHAPE_REPRESENTATION(#101,#11105);
#151=CONTEXT_DEPENDENT_SHAPE_REPRESENTATION(#102,#11106);
#152=CONTEXT_DEPENDENT_SHAPE_REPRESENTATION(#103,#11107);
#153=CONTEXT_DEPENDENT_SHAPE_REPRESENTATION(#104,#11108);
#154=CONTEXT_DEPENDENT_SHAPE_REPRESENTATION(#105,#11116);
#155=CONTEXT_DEPENDENT_SHAPE_REPRESENTATION(#106,#11117);
#156=CONTEXT_DEPENDENT_SHAPE_REPRESENTATION(#107,#11118);
#157=CONTEXT_DEPENDENT_SHAPE_REPRESENTATION(#108,#11119);
#158=CONTEXT_DEPENDENT_SHAPE_REPRESENTATION(#109,#11120);
#159=CONTEXT_DEPENDENT_SHAPE_REPRESENTATION(#110,#11121);
#160=CONTEXT_DEPENDENT_SHAPE_REPRESENTATION(#111,#11122);
#161=CONTEXT_DEPENDENT_SHAPE_REPRESENTATION(#112,#11123);
#162=CONTEXT_DEPENDENT_SHAPE_REPRESENTATION(#113,#11124);
#163=CONTEXT_DEPENDENT_SHAPE_REPRESENTATION(#114,#11125);
#164=CONTEXT_DEPENDENT_SHAPE_REPRESENTATION(#115,#11126);
#165=CONTEXT_DEPENDENT_SHAPE_REPRESENTATION(#116,#11127);
#166=CONTEXT_DEPENDENT_SHAPE_REPRESENTATION(#117,#11128);
#167=CONTEXT_DEPENDENT_SHAPE_REPRESENTATION(#118,#11129);
#168=CONTEXT_DEPENDENT_SHAPE_REPRESENTATION(#119,#11130);
#169=CONTEXT_DEPENDENT_SHAPE_REPRESENTATION(#120,#11131);
#170=CONTEXT_DEPENDENT_SHAPE_REPRESENTATION(#121,#11132);
#171=CONTEXT_DEPENDENT_SHAPE_REPRESENTATION(#122,#11133);
#172=CONTEXT_DEPENDENT_SHAPE_REPRESENTATION(#123,#11134);
#173=CONTEXT_DEPENDENT_SHAPE_REPRESENTATION(#124,#11135);
#174=CONTEXT_DEPENDENT_SHAPE_REPRESENTATION(#125,#11136);
#175=CONTEXT_DEPENDENT_SHAPE_REPRESENTATION(#126,#11137);
#176=CONTEXT_DEPENDENT_SHAPE_REPRESENTATION(#127,#11138);
#177=CONTEXT_DEPENDENT_SHAPE_REPRESENTATION(#128,#11139);
#178=CONTEXT_DEPENDENT_SHAPE_REPRESENTATION(#129,#11140);
#179=CONTEXT_DEPENDENT_SHAPE_REPRESENTATION(#130,#11141);
#180=CONTEXT_DEPENDENT_SHAPE_REPRESENTATION(#131,#11142);
#181=CONTEXT_DEPENDENT_SHAPE_REPRESENTATION(#132,#11143);
#182=CONTEXT_DEPENDENT_SHAPE_REPRESENTATION(#133,#11144);
#183=CONTEXT_DEPENDENT_SHAPE_REPRESENTATION(#134,#11145);
#184=CONTEXT_DEPENDENT_SHAPE_REPRESENTATION(#135,#11146);
#185=CONTEXT_DEPENDENT_SHAPE_REPRESENTATION(#136,#11147);
#186=CONTEXT_DEPENDENT_SHAPE_REPRESENTATION(#137,#11148);
#187=CONTEXT_DEPENDENT_SHAPE_REPRESENTATION(#138,#11149);
#188=CONTEXT_DEPENDENT_SHAPE_REPRESENTATION(#139,#11150);
#189=CONTEXT_DEPENDENT_SHAPE_REPRESENTATION(#140,#11151);
#190=CONTEXT_DEPENDENT_SHAPE_REPRESENTATION(#141,#11152);
#191=NEXT_ASSEMBLY_USAGE_OCCURRENCE('Steel sleeve:1','Steel sleeve:1',
'Steel sleeve:1',#11195,#11196,'Steel sleeve:1');
#192=NEXT_ASSEMBLY_USAGE_OCCURRENCE('Ball retainer (plastic):1',
'Ball retainer (plastic):1','Ball retainer (plastic):1',#11195,#11197,
'Ball retainer (plastic):1');
#193=NEXT_ASSEMBLY_USAGE_OCCURRENCE('Eccentric cam and spindle:1',
'Eccentric cam and spindle:1','Eccentric cam and spindle:1',#11199,#11200,
'Eccentric cam and spindle:1');
#194=NEXT_ASSEMBLY_USAGE_OCCURRENCE('Lower race sleeve:2',
'Lower race sleeve:2','Lower race sleeve:2',#11199,#11201,
'Lower race sleeve:2');
#195=NEXT_ASSEMBLY_USAGE_OCCURRENCE('Spindle collar:2',
'Spindle collar:2','Spindle collar:2',#11199,#11202,'Spindle collar:2');
#196=NEXT_ASSEMBLY_USAGE_OCCURRENCE('M4x4 collar screw:2',
'M4x4 collar screw:2','M4x4 collar screw:2',#11199,#11203,
'M4x4 collar screw:2');
#197=NEXT_ASSEMBLY_USAGE_OCCURRENCE('Forked roller follower:1',
'Forked roller follower:1','Forked roller follower:1',#11204,#11205,
'Forked roller follower:1');
#198=NEXT_ASSEMBLY_USAGE_OCCURRENCE('Roller axle:1','Roller axle:1',
'Roller axle:1',#11204,#11206,'Roller axle:1');
#199=NEXT_ASSEMBLY_USAGE_OCCURRENCE('Roller inner-race spacer:1',
'Roller inner-race spacer:1','Roller inner-race spacer:1',#11204,#11207,
'Roller inner-race spacer:1');
#200=NEXT_ASSEMBLY_USAGE_OCCURRENCE('Roller inner-race spacer (1):1',
'Roller inner-race spacer (1):1','Roller inner-race spacer (1):1',#11204,
#11208,'Roller inner-race spacer (1):1');
#201=NEXT_ASSEMBLY_USAGE_OCCURRENCE('Roller axle keeper:1',
'Roller axle keeper:1','Roller axle keeper:1',#11204,#11209,
'Roller axle keeper:1');
#202=NEXT_ASSEMBLY_USAGE_OCCURRENCE('M4x10 Cap Screw:14',
'M4x10 Cap Screw:14','M4x10 Cap Screw:14',#11204,#11210,
'M4x10 Cap Screw:14');
#203=NEXT_ASSEMBLY_USAGE_OCCURRENCE('Inner ring:1','Inner ring:1',
'Inner ring:1',#11212,#11213,'Inner ring:1');
#204=NEXT_ASSEMBLY_USAGE_OCCURRENCE('Outer ring:1','Outer ring:1',
'Outer ring:1',#11212,#11214,'Outer ring:1');
#205=NEXT_ASSEMBLY_USAGE_OCCURRENCE('Balls:1','Balls:1','Balls:1',#11212,
#11215,'Balls:1');
#206=NEXT_ASSEMBLY_USAGE_OCCURRENCE('Cage:1','Cage:1','Cage:1',#11212,#11216,
'Cage:1');
#207=NEXT_ASSEMBLY_USAGE_OCCURRENCE('Seals 2RS:1','Seals 2RS:1',
'Seals 2RS:1',#11212,#11217,'Seals 2RS:1');
#208=NEXT_ASSEMBLY_USAGE_OCCURRENCE('Cam demonstrator base:1',
'Cam demonstrator base:1','Cam demonstrator base:1',#11187,#11188,
'Cam demonstrator base:1');
#209=NEXT_ASSEMBLY_USAGE_OCCURRENCE('Linear follower guide:1',
'Linear follower guide:1','Linear follower guide:1',#11187,#11189,
'Linear follower guide:1');
#210=NEXT_ASSEMBLY_USAGE_OCCURRENCE('Linear guide retaining cap:1',
'Linear guide retaining cap:1','Linear guide retaining cap:1',#11187,#11190,
'Linear guide retaining cap:1');
#211=NEXT_ASSEMBLY_USAGE_OCCURRENCE('Linear guide retaining cap (1):1',
'Linear guide retaining cap (1):1','Linear guide retaining cap (1):1',#11187,
#11191,'Linear guide retaining cap (1):1');
#212=NEXT_ASSEMBLY_USAGE_OCCURRENCE('Installed follower spring:1',
'Installed follower spring:1','Installed follower spring:1',#11187,#11192,
'Installed follower spring:1');
#213=NEXT_ASSEMBLY_USAGE_OCCURRENCE('Pivot pedestal:2',
'Pivot pedestal:2','Pivot pedestal:2',#11187,#11193,'Pivot pedestal:2');
#214=NEXT_ASSEMBLY_USAGE_OCCURRENCE('Pivot cap:2','Pivot cap:2',
'Pivot cap:2',#11187,#11194,'Pivot cap:2');
#215=NEXT_ASSEMBLY_USAGE_OCCURRENCE(
'Sealed Ball Bearing - 10 x 30 x 9 mm:2',
'Sealed Ball Bearing - 10 x 30 x 9 mm:2',
'Sealed Ball Bearing - 10 x 30 x 9 mm:2',#11187,#11212,
'Sealed Ball Bearing - 10 x 30 x 9 mm:2');
#216=NEXT_ASSEMBLY_USAGE_OCCURRENCE('M5x14 Cap Screw:2',
'M5x14 Cap Screw:2','M5x14 Cap Screw:2',#11187,#11198,
'M5x14 Cap Screw:2');
#217=NEXT_ASSEMBLY_USAGE_OCCURRENCE('M4x10 Cap Screw:2',
'M4x10 Cap Screw:2','M4x10 Cap Screw:2',#11187,#11210,
'M4x10 Cap Screw:2');
#218=NEXT_ASSEMBLY_USAGE_OCCURRENCE('M5x14 Cap Screw:3',
'M5x14 Cap Screw:3','M5x14 Cap Screw:3',#11187,#11198,
'M5x14 Cap Screw:3');
#219=NEXT_ASSEMBLY_USAGE_OCCURRENCE('M4x10 Cap Screw:3',
'M4x10 Cap Screw:3','M4x10 Cap Screw:3',#11187,#11210,
'M4x10 Cap Screw:3');
#220=NEXT_ASSEMBLY_USAGE_OCCURRENCE('M5x14 Cap Screw:4',
'M5x14 Cap Screw:4','M5x14 Cap Screw:4',#11187,#11198,
'M5x14 Cap Screw:4');
#221=NEXT_ASSEMBLY_USAGE_OCCURRENCE('M4x10 Cap Screw:4',
'M4x10 Cap Screw:4','M4x10 Cap Screw:4',#11187,#11210,
'M4x10 Cap Screw:4');
#222=NEXT_ASSEMBLY_USAGE_OCCURRENCE('M5x14 Cap Screw:5',
'M5x14 Cap Screw:5','M5x14 Cap Screw:5',#11187,#11198,
'M5x14 Cap Screw:5');
#223=NEXT_ASSEMBLY_USAGE_OCCURRENCE('M4x10 Cap Screw:5',
'M4x10 Cap Screw:5','M4x10 Cap Screw:5',#11187,#11210,
'M4x10 Cap Screw:5');
#224=NEXT_ASSEMBLY_USAGE_OCCURRENCE(
'Linear Ball Bushing - 12 x 21 x 30 mm:2',
'Linear Ball Bushing - 12 x 21 x 30 mm:2',
'Linear Ball Bushing - 12 x 21 x 30 mm:2',#11187,#11195,
'Linear Ball Bushing - 12 x 21 x 30 mm:2');
#225=NEXT_ASSEMBLY_USAGE_OCCURRENCE('M5x14 Cap Screw:6',
'M5x14 Cap Screw:6','M5x14 Cap Screw:6',#11187,#11198,
'M5x14 Cap Screw:6');
#226=NEXT_ASSEMBLY_USAGE_OCCURRENCE('M5x14 Cap Screw:7',
'M5x14 Cap Screw:7','M5x14 Cap Screw:7',#11187,#11198,
'M5x14 Cap Screw:7');
#227=NEXT_ASSEMBLY_USAGE_OCCURRENCE('M4x10 Cap Screw:6',
'M4x10 Cap Screw:6','M4x10 Cap Screw:6',#11187,#11210,
'M4x10 Cap Screw:6');
#228=NEXT_ASSEMBLY_USAGE_OCCURRENCE('M4x10 Cap Screw:7',
'M4x10 Cap Screw:7','M4x10 Cap Screw:7',#11187,#11210,
'M4x10 Cap Screw:7');
#229=NEXT_ASSEMBLY_USAGE_OCCURRENCE('M4x10 Cap Screw:8',
'M4x10 Cap Screw:8','M4x10 Cap Screw:8',#11187,#11210,
'M4x10 Cap Screw:8');
#230=NEXT_ASSEMBLY_USAGE_OCCURRENCE('M4x10 Cap Screw:9',
'M4x10 Cap Screw:9','M4x10 Cap Screw:9',#11187,#11210,
'M4x10 Cap Screw:9');
#231=NEXT_ASSEMBLY_USAGE_OCCURRENCE('M4x10 Cap Screw:10',
'M4x10 Cap Screw:10','M4x10 Cap Screw:10',#11187,#11210,
'M4x10 Cap Screw:10');
#232=NEXT_ASSEMBLY_USAGE_OCCURRENCE('M4x10 Cap Screw:11',
'M4x10 Cap Screw:11','M4x10 Cap Screw:11',#11187,#11210,
'M4x10 Cap Screw:11');
#233=NEXT_ASSEMBLY_USAGE_OCCURRENCE('M4x10 Cap Screw:12',
'M4x10 Cap Screw:12','M4x10 Cap Screw:12',#11187,#11210,
'M4x10 Cap Screw:12');
#234=NEXT_ASSEMBLY_USAGE_OCCURRENCE('M4x10 Cap Screw:13',
'M4x10 Cap Screw:13','M4x10 Cap Screw:13',#11187,#11210,
'M4x10 Cap Screw:13');
#235=NEXT_ASSEMBLY_USAGE_OCCURRENCE(
'Sealed Ball Bearing - 10 x 30 x 9 mm:3',
'Sealed Ball Bearing - 10 x 30 x 9 mm:3',
'Sealed Ball Bearing - 10 x 30 x 9 mm:3',#11211,#11212,
'Sealed Ball Bearing - 10 x 30 x 9 mm:3');
#236=NEXT_ASSEMBLY_USAGE_OCCURRENCE('Base bearing and follower guide:1',
'Base bearing and follower guide:1','Base bearing and follower guide:1',
#11186,#11187,'Base bearing and follower guide:1');
#237=NEXT_ASSEMBLY_USAGE_OCCURRENCE('Eccentric cam spindle:1',
'Eccentric cam spindle:1','Eccentric cam spindle:1',#11186,#11199,
'Eccentric cam spindle:1');
#238=NEXT_ASSEMBLY_USAGE_OCCURRENCE('Guided follower and pin:1',
'Guided follower and pin:1','Guided follower and pin:1',#11186,#11204,
'Guided follower and pin:1');
#239=NEXT_ASSEMBLY_USAGE_OCCURRENCE('Bearing roller:1',
'Bearing roller:1','Bearing roller:1',#11186,#11211,'Bearing roller:1');
#240=B_SPLINE_SURFACE_WITH_KNOTS('',3,3,((#7917,#7918,#7919,#7920,#7921,
#7922,#7923,#7924,#7925,#7926,#7927,#7928,#7929,#7930,#7931,#7932,#7933,
#7934,#7935,#7936,#7937,#7938,#7939,#7940,#7941,#7942,#7943,#7944,#7945,
#7946,#7947,#7948,#7949,#7950,#7951,#7952,#7953,#7954,#7955,#7956,#7957,
#7958,#7959,#7960,#7961,#7962,#7963,#7964,#7965,#7966,#7967,#7968,#7969,
#7970,#7971,#7972,#7973,#7974,#7975,#7976,#7977,#7978,#7979,#7980,#7981,
#7982,#7983,#7984,#7985,#7986,#7987,#7988,#7989,#7990,#7991,#7992,#7993,
#7994,#7995,#7996,#7997,#7998,#7999,#8000,#8001,#8002,#8003,#8004,#8005,
#8006,#8007,#8008,#8009,#8010,#8011,#8012,#8013,#8014,#8015,#8016,#8017,
#8018,#8019,#8020,#8021,#8022,#8023,#8024,#8025,#8026,#8027,#8028,#8029,
#8030,#8031,#8032,#8033,#8034,#8035,#8036,#8037,#8038,#8039,#8040,#8041,
#8042,#8043,#8044,#8045,#8046,#8047,#8048,#8049,#8050,#8051,#8052,#8053,
#8054,#8055,#8056),(#8057,#8058,#8059,#8060,#8061,#8062,#8063,#8064,#8065,
#8066,#8067,#8068,#8069,#8070,#8071,#8072,#8073,#8074,#8075,#8076,#8077,
#8078,#8079,#8080,#8081,#8082,#8083,#8084,#8085,#8086,#8087,#8088,#8089,
#8090,#8091,#8092,#8093,#8094,#8095,#8096,#8097,#8098,#8099,#8100,#8101,
#8102,#8103,#8104,#8105,#8106,#8107,#8108,#8109,#8110,#8111,#8112,#8113,
#8114,#8115,#8116,#8117,#8118,#8119,#8120,#8121,#8122,#8123,#8124,#8125,
#8126,#8127,#8128,#8129,#8130,#8131,#8132,#8133,#8134,#8135,#8136,#8137,
#8138,#8139,#8140,#8141,#8142,#8143,#8144,#8145,#8146,#8147,#8148,#8149,
#8150,#8151,#8152,#8153,#8154,#8155,#8156,#8157,#8158,#8159,#8160,#8161,
#8162,#8163,#8164,#8165,#8166,#8167,#8168,#8169,#8170,#8171,#8172,#8173,
#8174,#8175,#8176,#8177,#8178,#8179,#8180,#8181,#8182,#8183,#8184,#8185,
#8186,#8187,#8188,#8189,#8190,#8191,#8192,#8193,#8194,#8195,#8196),(#8197,
#8198,#8199,#8200,#8201,#8202,#8203,#8204,#8205,#8206,#8207,#8208,#8209,
#8210,#8211,#8212,#8213,#8214,#8215,#8216,#8217,#8218,#8219,#8220,#8221,
#8222,#8223,#8224,#8225,#8226,#8227,#8228,#8229,#8230,#8231,#8232,#8233,
#8234,#8235,#8236,#8237,#8238,#8239,#8240,#8241,#8242,#8243,#8244,#8245,
#8246,#8247,#8248,#8249,#8250,#8251,#8252,#8253,#8254,#8255,#8256,#8257,
#8258,#8259,#8260,#8261,#8262,#8263,#8264,#8265,#8266,#8267,#8268,#8269,
#8270,#8271,#8272,#8273,#8274,#8275,#8276,#8277,#8278,#8279,#8280,#8281,
#8282,#8283,#8284,#8285,#8286,#8287,#8288,#8289,#8290,#8291,#8292,#8293,
#8294,#8295,#8296,#8297,#8298,#8299,#8300,#8301,#8302,#8303,#8304,#8305,
#8306,#8307,#8308,#8309,#8310,#8311,#8312,#8313,#8314,#8315,#8316,#8317,
#8318,#8319,#8320,#8321,#8322,#8323,#8324,#8325,#8326,#8327,#8328,#8329,
#8330,#8331,#8332,#8333,#8334,#8335,#8336),(#8337,#8338,#8339,#8340,#8341,
#8342,#8343,#8344,#8345,#8346,#8347,#8348,#8349,#8350,#8351,#8352,#8353,
#8354,#8355,#8356,#8357,#8358,#8359,#8360,#8361,#8362,#8363,#8364,#8365,
#8366,#8367,#8368,#8369,#8370,#8371,#8372,#8373,#8374,#8375,#8376,#8377,
#8378,#8379,#8380,#8381,#8382,#8383,#8384,#8385,#8386,#8387,#8388,#8389,
#8390,#8391,#8392,#8393,#8394,#8395,#8396,#8397,#8398,#8399,#8400,#8401,
#8402,#8403,#8404,#8405,#8406,#8407,#8408,#8409,#8410,#8411,#8412,#8413,
#8414,#8415,#8416,#8417,#8418,#8419,#8420,#8421,#8422,#8423,#8424,#8425,
#8426,#8427,#8428,#8429,#8430,#8431,#8432,#8433,#8434,#8435,#8436,#8437,
#8438,#8439,#8440,#8441,#8442,#8443,#8444,#8445,#8446,#8447,#8448,#8449,
#8450,#8451,#8452,#8453,#8454,#8455,#8456,#8457,#8458,#8459,#8460,#8461,
#8462,#8463,#8464,#8465,#8466,#8467,#8468,#8469,#8470,#8471,#8472,#8473,
#8474,#8475,#8476),(#8477,#8478,#8479,#8480,#8481,#8482,#8483,#8484,#8485,
#8486,#8487,#8488,#8489,#8490,#8491,#8492,#8493,#8494,#8495,#8496,#8497,
#8498,#8499,#8500,#8501,#8502,#8503,#8504,#8505,#8506,#8507,#8508,#8509,
#8510,#8511,#8512,#8513,#8514,#8515,#8516,#8517,#8518,#8519,#8520,#8521,
#8522,#8523,#8524,#8525,#8526,#8527,#8528,#8529,#8530,#8531,#8532,#8533,
#8534,#8535,#8536,#8537,#8538,#8539,#8540,#8541,#8542,#8543,#8544,#8545,
#8546,#8547,#8548,#8549,#8550,#8551,#8552,#8553,#8554,#8555,#8556,#8557,
#8558,#8559,#8560,#8561,#8562,#8563,#8564,#8565,#8566,#8567,#8568,#8569,
#8570,#8571,#8572,#8573,#8574,#8575,#8576,#8577,#8578,#8579,#8580,#8581,
#8582,#8583,#8584,#8585,#8586,#8587,#8588,#8589,#8590,#8591,#8592,#8593,
#8594,#8595,#8596,#8597,#8598,#8599,#8600,#8601,#8602,#8603,#8604,#8605,
#8606,#8607,#8608,#8609,#8610,#8611,#8612,#8613,#8614,#8615,#8616),(#8617,
#8618,#8619,#8620,#8621,#8622,#8623,#8624,#8625,#8626,#8627,#8628,#8629,
#8630,#8631,#8632,#8633,#8634,#8635,#8636,#8637,#8638,#8639,#8640,#8641,
#8642,#8643,#8644,#8645,#8646,#8647,#8648,#8649,#8650,#8651,#8652,#8653,
#8654,#8655,#8656,#8657,#8658,#8659,#8660,#8661,#8662,#8663,#8664,#8665,
#8666,#8667,#8668,#8669,#8670,#8671,#8672,#8673,#8674,#8675,#8676,#8677,
#8678,#8679,#8680,#8681,#8682,#8683,#8684,#8685,#8686,#8687,#8688,#8689,
#8690,#8691,#8692,#8693,#8694,#8695,#8696,#8697,#8698,#8699,#8700,#8701,
#8702,#8703,#8704,#8705,#8706,#8707,#8708,#8709,#8710,#8711,#8712,#8713,
#8714,#8715,#8716,#8717,#8718,#8719,#8720,#8721,#8722,#8723,#8724,#8725,
#8726,#8727,#8728,#8729,#8730,#8731,#8732,#8733,#8734,#8735,#8736,#8737,
#8738,#8739,#8740,#8741,#8742,#8743,#8744,#8745,#8746,#8747,#8748,#8749,
#8750,#8751,#8752,#8753,#8754,#8755,#8756),(#8757,#8758,#8759,#8760,#8761,
#8762,#8763,#8764,#8765,#8766,#8767,#8768,#8769,#8770,#8771,#8772,#8773,
#8774,#8775,#8776,#8777,#8778,#8779,#8780,#8781,#8782,#8783,#8784,#8785,
#8786,#8787,#8788,#8789,#8790,#8791,#8792,#8793,#8794,#8795,#8796,#8797,
#8798,#8799,#8800,#8801,#8802,#8803,#8804,#8805,#8806,#8807,#8808,#8809,
#8810,#8811,#8812,#8813,#8814,#8815,#8816,#8817,#8818,#8819,#8820,#8821,
#8822,#8823,#8824,#8825,#8826,#8827,#8828,#8829,#8830,#8831,#8832,#8833,
#8834,#8835,#8836,#8837,#8838,#8839,#8840,#8841,#8842,#8843,#8844,#8845,
#8846,#8847,#8848,#8849,#8850,#8851,#8852,#8853,#8854,#8855,#8856,#8857,
#8858,#8859,#8860,#8861,#8862,#8863,#8864,#8865,#8866,#8867,#8868,#8869,
#8870,#8871,#8872,#8873,#8874,#8875,#8876,#8877,#8878,#8879,#8880,#8881,
#8882,#8883,#8884,#8885,#8886,#8887,#8888,#8889,#8890,#8891,#8892,#8893,
#8894,#8895,#8896),(#8897,#8898,#8899,#8900,#8901,#8902,#8903,#8904,#8905,
#8906,#8907,#8908,#8909,#8910,#8911,#8912,#8913,#8914,#8915,#8916,#8917,
#8918,#8919,#8920,#8921,#8922,#8923,#8924,#8925,#8926,#8927,#8928,#8929,
#8930,#8931,#8932,#8933,#8934,#8935,#8936,#8937,#8938,#8939,#8940,#8941,
#8942,#8943,#8944,#8945,#8946,#8947,#8948,#8949,#8950,#8951,#8952,#8953,
#8954,#8955,#8956,#8957,#8958,#8959,#8960,#8961,#8962,#8963,#8964,#8965,
#8966,#8967,#8968,#8969,#8970,#8971,#8972,#8973,#8974,#8975,#8976,#8977,
#8978,#8979,#8980,#8981,#8982,#8983,#8984,#8985,#8986,#8987,#8988,#8989,
#8990,#8991,#8992,#8993,#8994,#8995,#8996,#8997,#8998,#8999,#9000,#9001,
#9002,#9003,#9004,#9005,#9006,#9007,#9008,#9009,#9010,#9011,#9012,#9013,
#9014,#9015,#9016,#9017,#9018,#9019,#9020,#9021,#9022,#9023,#9024,#9025,
#9026,#9027,#9028,#9029,#9030,#9031,#9032,#9033,#9034,#9035,#9036),(#9037,
#9038,#9039,#9040,#9041,#9042,#9043,#9044,#9045,#9046,#9047,#9048,#9049,
#9050,#9051,#9052,#9053,#9054,#9055,#9056,#9057,#9058,#9059,#9060,#9061,
#9062,#9063,#9064,#9065,#9066,#9067,#9068,#9069,#9070,#9071,#9072,#9073,
#9074,#9075,#9076,#9077,#9078,#9079,#9080,#9081,#9082,#9083,#9084,#9085,
#9086,#9087,#9088,#9089,#9090,#9091,#9092,#9093,#9094,#9095,#9096,#9097,
#9098,#9099,#9100,#9101,#9102,#9103,#9104,#9105,#9106,#9107,#9108,#9109,
#9110,#9111,#9112,#9113,#9114,#9115,#9116,#9117,#9118,#9119,#9120,#9121,
#9122,#9123,#9124,#9125,#9126,#9127,#9128,#9129,#9130,#9131,#9132,#9133,
#9134,#9135,#9136,#9137,#9138,#9139,#9140,#9141,#9142,#9143,#9144,#9145,
#9146,#9147,#9148,#9149,#9150,#9151,#9152,#9153,#9154,#9155,#9156,#9157,
#9158,#9159,#9160,#9161,#9162,#9163,#9164,#9165,#9166,#9167,#9168,#9169,
#9170,#9171,#9172,#9173,#9174,#9175,#9176),(#9177,#9178,#9179,#9180,#9181,
#9182,#9183,#9184,#9185,#9186,#9187,#9188,#9189,#9190,#9191,#9192,#9193,
#9194,#9195,#9196,#9197,#9198,#9199,#9200,#9201,#9202,#9203,#9204,#9205,
#9206,#9207,#9208,#9209,#9210,#9211,#9212,#9213,#9214,#9215,#9216,#9217,
#9218,#9219,#9220,#9221,#9222,#9223,#9224,#9225,#9226,#9227,#9228,#9229,
#9230,#9231,#9232,#9233,#9234,#9235,#9236,#9237,#9238,#9239,#9240,#9241,
#9242,#9243,#9244,#9245,#9246,#9247,#9248,#9249,#9250,#9251,#9252,#9253,
#9254,#9255,#9256,#9257,#9258,#9259,#9260,#9261,#9262,#9263,#9264,#9265,
#9266,#9267,#9268,#9269,#9270,#9271,#9272,#9273,#9274,#9275,#9276,#9277,
#9278,#9279,#9280,#9281,#9282,#9283,#9284,#9285,#9286,#9287,#9288,#9289,
#9290,#9291,#9292,#9293,#9294,#9295,#9296,#9297,#9298,#9299,#9300,#9301,
#9302,#9303,#9304,#9305,#9306,#9307,#9308,#9309,#9310,#9311,#9312,#9313,
#9314,#9315,#9316)),.UNSPECIFIED.,.T.,.F.,.F.,(4,1,1,1,1,1,1,4),(4,1,1,
1,1,1,1,1,1,1,1,1,1,1,1,1,1,1,1,1,1,1,1,1,1,1,1,1,1,1,1,1,1,1,1,1,1,1,1,
1,1,1,1,1,1,1,1,1,1,1,1,1,1,1,1,1,1,1,1,1,1,1,1,1,1,1,1,1,1,1,1,1,1,1,1,
1,1,1,1,1,1,1,1,1,1,1,1,1,1,1,1,1,1,1,1,1,1,1,1,1,1,1,1,1,1,1,1,1,1,1,1,
1,1,1,1,1,1,1,1,1,1,1,1,1,1,1,1,1,1,1,1,1,1,1,1,1,1,4),(-3.14159265358979,
-2.24399475256414,-1.34639685153848,-0.448798950512828,0.448798950512828,
1.34639685153848,2.24399475256414,3.14159265358979),(0.,0.00892857142857143,
0.0178571428571429,0.0267857142857143,0.0357142857142857,0.0446428571428571,
0.0535714285714286,0.0625,0.0714285714285714,0.0758928571428571,0.0803571428571428,
0.0848214285714286,0.0892857142857143,0.09375,0.0948660714285714,0.0959821428571428,
0.0970982142857143,0.0982142857142857,0.100446428571429,0.102678571428571,
0.107142857142857,0.116071428571429,0.120535714285714,0.125,0.133928571428571,
0.142857142857143,0.150793650793651,0.158730158730159,0.166666666666667,
0.174603174603175,0.182539682539683,0.19047619047619,0.196428571428571,
0.202380952380952,0.214285714285714,0.222222222222222,0.23015873015873,
0.238095238095238,0.241071428571429,0.244047619047619,0.25,0.261904761904762,
0.273809523809524,0.285714285714286,0.297619047619048,0.30952380952381,
0.321428571428571,0.327380952380952,0.333333333333333,0.341269841269841,
0.349206349206349,0.357142857142857,0.361111111111111,0.365079365079365,
0.373015873015873,0.380952380952381,0.392857142857143,0.398809523809524,
0.404761904761905,0.416666666666667,0.428571428571429,0.4375,0.446428571428571,
0.455357142857143,0.457589285714286,0.459821428571429,0.462053571428571,
0.464285714285714,0.470238095238095,0.482142857142857,0.491071428571429,
0.5,0.508928571428571,0.517857142857143,0.526785714285714,0.535714285714286,
0.544642857142857,0.553571428571429,0.5625,0.571428571428571,0.580357142857143,
0.589285714285714,0.598214285714286,0.607142857142857,0.616071428571429,
0.625,0.633928571428571,0.638392857142857,0.642857142857143,0.650793650793651,
0.658730158730159,0.666666666666667,0.672619047619048,0.678571428571428,
0.69047619047619,0.702380952380952,0.714285714285714,0.726190476190476,
0.738095238095238,0.744047619047619,0.75,0.761904761904762,0.76984126984127,
0.777777777777778,0.785714285714286,0.794642857142857,0.803571428571428,
0.8125,0.821428571428571,0.830357142857143,0.839285714285714,0.848214285714286,
0.857142857142857,0.866071428571429,0.875,0.879464285714286,0.883928571428571,
0.892857142857143,0.897321428571428,0.899553571428571,0.901785714285714,
0.902901785714286,0.904017857142857,0.905133928571429,0.90625,0.910714285714286,
0.915178571428571,0.919642857142857,0.924107142857143,0.928571428571429,
0.9375,0.946428571428571,0.955357142857143,0.964285714285714,0.973214285714286,
0.982142857142857,0.991071428571429,1.),.UNSPECIFIED.);
#241=B_SPLINE_CURVE_WITH_KNOTS('',3,(#7321,#7322,#7323,#7324,#7325,#7326,
#7327,#7328,#7329,#7330,#7331,#7332,#7333,#7334,#7335,#7336,#7337,#7338,
#7339,#7340,#7341,#7342,#7343,#7344,#7345,#7346,#7347,#7348,#7349,#7350),
 .UNSPECIFIED.,.F.,.F.,(4,2,2,2,2,2,2,2,2,2,2,2,2,2,4),(0.,0.0614386993115687,
0.122877398623137,0.194452004299172,0.266026609975207,0.361453659820112,
0.456880709665017,0.528368337752035,0.564112151795545,0.599855965839054,
0.635599779882563,0.671343593926072,0.742831222013091,0.838258271857996,
0.933685321702901),.UNSPECIFIED.);
#242=B_SPLINE_CURVE_WITH_KNOTS('',3,(#7351,#7352,#7353,#7354,#7355,#7356,
#7357,#7358,#7359,#7360),.UNSPECIFIED.,.F.,.F.,(4,2,2,2,4),(0.933685321702901,
1.00525992737894,1.07683453305497,1.13827323236654,1.19971193167811),
 .UNSPECIFIED.);
#243=B_SPLINE_CURVE_WITH_KNOTS('',3,(#7364,#7365,#7366,#7367,#7368,#7369,
#7370,#7371,#7372,#7373),.UNSPECIFIED.,.F.,.F.,(4,2,2,2,4),(0.,0.061438699311569,
0.122877398623138,0.194452004299173,0.266026609975207),.UNSPECIFIED.);
#244=B_SPLINE_CURVE_WITH_KNOTS('',3,(#7374,#7375,#7376,#7377,#7378,#7379,
#7380,#7381,#7382,#7383,#7384,#7385,#7386,#7387,#7388,#7389,#7390,#7391,
#7392,#7393,#7394,#7395,#7396,#7397,#7398,#7399,#7400,#7401,#7402,#7403),
 .UNSPECIFIED.,.F.,.F.,(4,2,2,2,2,2,2,2,2,2,2,2,2,2,4),(0.266026609975207,
0.361453659820112,0.456880709665017,0.528368337752036,0.564112151795545,
0.599855965839054,0.635599779882563,0.671343593926073,0.742831222013091,
0.838258271857996,0.933685321702901,1.00525992737894,1.07683453305497,1.13827323236654,
1.19971193167811),.UNSPECIFIED.);
#245=B_SPLINE_CURVE_WITH_KNOTS('',3,(#7413,#7414,#7415,#7416,#7417,#7418,
#7419,#7420,#7421,#7422,#7423,#7424,#7425,#7426,#7427,#7428,#7429,#7430,
#7431,#7432,#7433,#7434,#7435,#7436,#7437,#7438,#7439,#7440),
 .UNSPECIFIED.,.F.,.F.,(4,2,2,2,2,2,2,2,2,2,2,2,2,4),(0.,0.028138639371576,
0.0562772787431521,0.154843288866037,0.240109193198138,0.325375097530239,
0.395403587057064,0.46543207658389,0.528409281202622,0.591386485821355,
0.652825185132924,0.714263884444493,0.785838490120527,0.857413095796562),
 .UNSPECIFIED.);
#246=B_SPLINE_CURVE_WITH_KNOTS('',3,(#7441,#7442,#7443,#7444,#7445,#7446,
#7447,#7448,#7449,#7450,#7451,#7452),.UNSPECIFIED.,.F.,.F.,(4,2,2,2,2,4),
(0.857413095796562,0.952840145641466,1.04826719548637,1.11975482357339,
1.1554986376169,1.19124245166041),.UNSPECIFIED.);
#247=B_SPLINE_CURVE_WITH_KNOTS('',3,(#7456,#7457,#7458,#7459,#7460,#7461,
#7462,#7463,#7464,#7465,#7466,#7467),.UNSPECIFIED.,.F.,.F.,(4,2,2,2,2,4),
(0.,0.0357438140435093,0.0714876280870186,0.142975256174037,0.238402306018942,
0.333829355863846),.UNSPECIFIED.);
#248=B_SPLINE_CURVE_WITH_KNOTS('',3,(#7468,#7469,#7470,#7471,#7472,#7473,
#7474,#7475,#7476,#7477,#7478,#7479,#7480,#7481,#7482,#7483,#7484,#7485,
#7486,#7487,#7488,#7489,#7490,#7491,#7492,#7493,#7494,#7495),
 .UNSPECIFIED.,.F.,.F.,(4,2,2,2,2,2,2,2,2,2,2,2,2,4),(0.333829355863846,
0.40540396153988,0.476978567215915,0.538417266527484,0.599855965839053,
0.662833170457785,0.725810375076518,0.795838864603343,0.865867354130168,
0.951133258462269,1.03639916279437,1.13496517291726,1.16310381228883,1.19124245166041),
 .UNSPECIFIED.);
#249=B_SPLINE_CURVE_WITH_KNOTS('',3,(#7505,#7506,#7507,#7508,#7509,#7510,
#7511,#7512,#7513,#7514,#7515,#7516,#7517,#7518,#7519,#7520,#7521,#7522,
#7523,#7524,#7525,#7526,#7527,#7528,#7529,#7530,#7531,#7532),
 .UNSPECIFIED.,.F.,.F.,(4,2,2,2,2,2,2,2,2,2,2,2,2,4),(0.,0.0357438140435092,
0.0714876280870185,0.142975256174037,0.238402306018942,0.333829355863847,
0.405403961539882,0.476978567215916,0.538417266527485,0.599855965839054,
0.661294665150623,0.722733364462192,0.794307970138227,0.865882575814261),
 .UNSPECIFIED.);
#250=B_SPLINE_CURVE_WITH_KNOTS('',3,(#7533,#7534,#7535,#7536,#7537,#7538,
#7539,#7540,#7541,#7542,#7543,#7544),.UNSPECIFIED.,.F.,.F.,(4,2,2,2,2,4),
(0.865882575814261,0.961309625659166,1.05673667550407,1.12822430359109,
1.1639681176346,1.19971193167811),.UNSPECIFIED.);
#251=B_SPLINE_CURVE_WITH_KNOTS('',3,(#7548,#7549,#7550,#7551,#7552,#7553,
#7554,#7555,#7556,#7557,#7558,#7559),.UNSPECIFIED.,.F.,.F.,(4,2,2,2,2,4),
(0.,0.0357438140435093,0.0714876280870185,0.142975256174037,0.238402306018942,
0.333829355863847),.UNSPECIFIED.);
#252=B_SPLINE_CURVE_WITH_KNOTS('',3,(#7560,#7561,#7562,#7563,#7564,#7565,
#7566,#7567,#7568,#7569,#7570,#7571,#7572,#7573,#7574,#7575,#7576,#7577,
#7578,#7579,#7580,#7581,#7582,#7583,#7584,#7585,#7586,#7587),
 .UNSPECIFIED.,.F.,.F.,(4,2,2,2,2,2,2,2,2,2,2,2,2,4),(0.333829355863847,
0.405403961539881,0.476978567215916,0.538417266527485,0.599855965839054,
0.661294665150623,0.722733364462191,0.794307970138226,0.865882575814261,
0.961309625659166,1.05673667550407,1.12822430359109,1.1639681176346,1.19971193167811),
 .UNSPECIFIED.);
#253=B_SPLINE_CURVE_WITH_KNOTS('',3,(#7597,#7598,#7599,#7600,#7601,#7602,
#7603,#7604,#7605,#7606,#7607,#7608,#7609,#7610,#7611,#7612,#7613,#7614,
#7615,#7616,#7617,#7618,#7619,#7620,#7621,#7622,#7623,#7624,#7625,#7626),
 .UNSPECIFIED.,.F.,.F.,(4,2,2,2,2,2,2,2,2,2,2,2,2,2,4),(0.,0.0629772046187326,
0.125954409237465,0.195982898764291,0.266011388291116,0.351277292623217,
0.436543196955317,0.535109207078203,0.563247846449779,0.591386485821355,
0.627130299864864,0.662874113908373,0.734361741995392,0.829788791840296,
0.925215841685201),.UNSPECIFIED.);
#254=B_SPLINE_CURVE_WITH_KNOTS('',3,(#7627,#7628,#7629,#7630,#7631,#7632,
#7633,#7634,#7635,#7636),.UNSPECIFIED.,.F.,.F.,(4,2,2,2,4),(0.925215841685201,
0.996790447361235,1.06836505303727,1.12980375234884,1.19124245166041),
 .UNSPECIFIED.);
#255=B_SPLINE_CURVE_WITH_KNOTS('',3,(#7640,#7641,#7642,#7643,#7644,#7645,
#7646,#7647,#7648,#7649),.UNSPECIFIED.,.F.,.F.,(4,2,2,2,4),(0.,0.061438699311569,
0.122877398623138,0.194452004299172,0.266026609975207),.UNSPECIFIED.);
#256=B_SPLINE_CURVE_WITH_KNOTS('',3,(#7650,#7651,#7652,#7653,#7654,#7655,
#7656,#7657,#7658,#7659,#7660,#7661,#7662,#7663,#7664,#7665,#7666,#7667,
#7668,#7669,#7670,#7671,#7672,#7673,#7674,#7675,#7676,#7677,#7678,#7679),
 .UNSPECIFIED.,.F.,.F.,(4,2,2,2,2,2,2,2,2,2,2,2,2,2,4),(0.266026609975207,
0.361453659820111,0.456880709665016,0.528368337752034,0.564112151795544,
0.599855965839053,0.627994605210629,0.656133244582205,0.75469925470509,
0.839965159037191,0.925231063369292,0.995259552896117,1.06528804242294,
1.12826524704167,1.19124245166041),.UNSPECIFIED.);
#257=B_SPLINE_CURVE_WITH_KNOTS('',3,(#7688,#7689,#7690,#7691,#7692,#7693,
#7694,#7695,#7696,#7697,#7698,#7699,#7700,#7701,#7702,#7703,#7704,#7705,
#7706,#7707,#7708,#7709,#7710,#7711,#7712,#7713,#7714,#7715,#7716,#7717,
#7718,#7719,#7720,#7721,#7722,#7723,#7724,#7725,#7726,#7727,#7728,#7729),
 .UNSPECIFIED.,.T.,.F.,(4,2,2,2,2,2,2,2,2,2,2,2,2,2,2,2,2,2,2,2,4),(0.,
0.157447434703095,0.236171152054642,0.314894869406189,0.367076252690622,
0.419257635975055,0.471439019259488,0.523620402543921,0.602344119895468,
0.681067837247015,0.83851527195011,0.995962706653205,1.07468642400475,1.1534101413563,
1.20559152464073,1.25777290792516,1.3099542912096,1.36213567449403,1.44085939184558,
1.51958310919713,1.67703054390022),.UNSPECIFIED.);
#258=B_SPLINE_CURVE_WITH_KNOTS('',3,(#7742,#7743,#7744,#7745,#7746,#7747,
#7748,#7749,#7750,#7751,#7752,#7753,#7754,#7755,#7756,#7757,#7758,#7759,
#7760,#7761,#7762,#7763,#7764,#7765,#7766,#7767,#7768,#7769,#7770,#7771,
#7772,#7773,#7774,#7775,#7776,#7777,#7778,#7779,#7780,#7781,#7782,#7783),
 .UNSPECIFIED.,.T.,.F.,(4,2,2,2,2,2,2,2,2,2,2,2,2,2,2,2,2,2,2,2,4),(0.,
0.157447434703095,0.236171152054642,0.314894869406189,0.367076252690622,
0.419257635975055,0.471439019259488,0.523620402543921,0.602344119895468,
0.681067837247015,0.83851527195011,0.995962706653205,1.07468642400475,1.1534101413563,
1.20559152464073,1.25777290792516,1.3099542912096,1.36213567449403,1.44085939184558,
1.51958310919713,1.67703054390022),.UNSPECIFIED.);
#259=B_SPLINE_CURVE_WITH_KNOTS('',3,(#9320,#9321,#9322,#9323,#9324,#9325,
#9326,#9327,#9328,#9329,#9330,#9331,#9332,#9333,#9334,#9335,#9336,#9337,
#9338,#9339,#9340,#9341,#9342,#9343,#9344,#9345,#9346,#9347,#9348,#9349,
#9350,#9351,#9352,#9353,#9354,#9355,#9356,#9357,#9358,#9359,#9360,#9361,
#9362,#9363,#9364,#9365,#9366,#9367,#9368,#9369,#9370,#9371,#9372,#9373,
#9374,#9375,#9376,#9377,#9378,#9379,#9380,#9381,#9382,#9383,#9384,#9385,
#9386,#9387,#9388,#9389,#9390,#9391,#9392,#9393,#9394,#9395,#9396,#9397,
#9398,#9399,#9400,#9401,#9402,#9403,#9404,#9405,#9406,#9407,#9408,#9409,
#9410,#9411,#9412,#9413,#9414,#9415,#9416,#9417,#9418,#9419,#9420,#9421,
#9422,#9423,#9424,#9425,#9426,#9427,#9428,#9429,#9430,#9431,#9432,#9433,
#9434,#9435,#9436,#9437,#9438,#9439,#9440,#9441,#9442,#9443,#9444,#9445,
#9446,#9447,#9448,#9449,#9450,#9451,#9452,#9453,#9454,#9455,#9456,#9457,
#9458,#9459),.UNSPECIFIED.,.F.,.F.,(4,1,1,1,1,1,1,1,1,1,1,1,1,1,1,1,1,1,
1,1,1,1,1,1,1,1,1,1,1,1,1,1,1,1,1,1,1,1,1,1,1,1,1,1,1,1,1,1,1,1,1,1,1,1,
1,1,1,1,1,1,1,1,1,1,1,1,1,1,1,1,1,1,1,1,1,1,1,1,1,1,1,1,1,1,1,1,1,1,1,1,
1,1,1,1,1,1,1,1,1,1,1,1,1,1,1,1,1,1,1,1,1,1,1,1,1,1,1,1,1,1,1,1,1,1,1,1,
1,1,1,1,1,1,1,1,1,1,1,4),(0.,0.00892857142857143,0.0178571428571429,0.0267857142857143,
0.0357142857142857,0.0446428571428571,0.0535714285714286,0.0625,0.0714285714285714,
0.0758928571428571,0.0803571428571428,0.0848214285714286,0.0892857142857143,
0.09375,0.0948660714285714,0.0959821428571428,0.0970982142857143,0.0982142857142857,
0.100446428571429,0.102678571428571,0.107142857142857,0.116071428571429,
0.120535714285714,0.125,0.133928571428571,0.142857142857143,0.150793650793651,
0.158730158730159,0.166666666666667,0.174603174603175,0.182539682539683,
0.19047619047619,0.196428571428571,0.202380952380952,0.214285714285714,
0.222222222222222,0.23015873015873,0.238095238095238,0.241071428571429,
0.244047619047619,0.25,0.261904761904762,0.273809523809524,0.285714285714286,
0.297619047619048,0.30952380952381,0.321428571428571,0.327380952380952,
0.333333333333333,0.341269841269841,0.349206349206349,0.357142857142857,
0.361111111111111,0.365079365079365,0.373015873015873,0.380952380952381,
0.392857142857143,0.398809523809524,0.404761904761905,0.416666666666667,
0.428571428571429,0.4375,0.446428571428571,0.455357142857143,0.457589285714286,
0.459821428571429,0.462053571428571,0.464285714285714,0.470238095238095,
0.482142857142857,0.491071428571429,0.5,0.508928571428571,0.517857142857143,
0.526785714285714,0.535714285714286,0.544642857142857,0.553571428571429,
0.5625,0.571428571428571,0.580357142857143,0.589285714285714,0.598214285714286,
0.607142857142857,0.616071428571429,0.625,0.633928571428571,0.638392857142857,
0.642857142857143,0.650793650793651,0.658730158730159,0.666666666666667,
0.672619047619048,0.678571428571428,0.69047619047619,0.702380952380952,
0.714285714285714,0.726190476190476,0.738095238095238,0.744047619047619,
0.75,0.761904761904762,0.76984126984127,0.777777777777778,0.785714285714286,
0.794642857142857,0.803571428571428,0.8125,0.821428571428571,0.830357142857143,
0.839285714285714,0.848214285714286,0.857142857142857,0.866071428571429,
0.875,0.879464285714286,0.883928571428571,0.892857142857143,0.897321428571428,
0.899553571428571,0.901785714285714,0.902901785714286,0.904017857142857,
0.905133928571429,0.90625,0.910714285714286,0.915178571428571,0.919642857142857,
0.924107142857143,0.928571428571429,0.9375,0.946428571428571,0.955357142857143,
0.964285714285714,0.973214285714286,0.982142857142857,0.991071428571429,
1.),.UNSPECIFIED.);
#260=B_SPLINE_CURVE_WITH_KNOTS('',3,(#9467,#9468,#9469,#9470,#9471,#9472,
#9473,#9474,#9475,#9476),.UNSPECIFIED.,.F.,.F.,(4,2,2,2,4),(0.,0.0945941824764479,
0.189188364952896,0.283770357603024,0.378352350253152),.UNSPECIFIED.);
#261=B_SPLINE_CURVE_WITH_KNOTS('',3,(#9477,#9478,#9479,#9480,#9481,#9482,
#9483,#9484,#9485,#9486,#9487,#9488,#9489,#9490,#9491,#9492,#9493,#9494,
#9495,#9496,#9497,#9498,#9499,#9500,#9501,#9502),.UNSPECIFIED.,.F.,.F.,
(4,2,2,2,2,2,2,2,2,2,2,2,4),(0.378352350253152,0.47293434290328,0.567516335553408,
0.662110518029855,0.756704700506303,0.851298882982751,0.945893065459199,
1.04047505810933,1.13505705075946,1.22963904340958,1.32422103605971,1.41881521853616,
1.51340940101261),.UNSPECIFIED.);
#262=B_SPLINE_CURVE_WITH_KNOTS('',3,(#9506,#9507,#9508,#9509,#9510,#9511,
#9512,#9513,#9514,#9515,#9516,#9517,#9518,#9519,#9520,#9521,#9522,#9523,
#9524,#9525,#9526,#9527,#9528,#9529,#9530,#9531),.UNSPECIFIED.,.F.,.F.,
(4,2,2,2,2,2,2,2,2,2,2,2,4),(0.,0.0942186410044058,0.188437282008812,0.282655768798837,
0.376874255588861,0.471092742378886,0.565311229168911,0.659529870173317,
0.753748511177723,0.847967152182129,0.942185793186535,1.03640427997656,
1.13062276676658),.UNSPECIFIED.);
#263=B_SPLINE_CURVE_WITH_KNOTS('',3,(#9532,#9533,#9534,#9535,#9536,#9537,
#9538,#9539,#9540,#9541),.UNSPECIFIED.,.F.,.F.,(4,2,2,2,4),(1.13062276676658,
1.22484125355661,1.31905974034663,1.41327838135104,1.50749702235545),
 .UNSPECIFIED.);
#264=B_SPLINE_CURVE_WITH_KNOTS('',3,(#9974,#9975,#9976,#9977,#9978,#9979,
#9980,#9981,#9982,#9983,#9984,#9985,#9986,#9987),.UNSPECIFIED.,.F.,.F.,
(4,2,2,2,2,2,4),(0.618551524396293,0.626563103102765,0.689203386094988,
0.751843669087211,0.814483952079434,0.877124235071657,0.88513581377813),
 .UNSPECIFIED.);
#265=B_SPLINE_CURVE_WITH_KNOTS('',3,(#9991,#9992,#9993,#9994,#9995,#9996,
#9997,#9998),.UNSPECIFIED.,.F.,.F.,(4,2,2,4),(0.250614556362404,0.313254839354627,
0.37589512234685,0.383906701053323),.UNSPECIFIED.);
#266=B_SPLINE_CURVE_WITH_KNOTS('',3,(#10002,#10003,#10004,#10005,#10006,
#10007,#10008,#10009,#10010,#10011,#10012,#10013,#10014,#10015,#10016,#10017,
#10018,#10019,#10020,#10021,#10022,#10023,#10024,#10025,#10026,#10027),
 .UNSPECIFIED.,.F.,.F.,(4,2,2,2,2,2,2,2,2,2,2,2,4),(0.,0.0623062782223143,
0.124612556444629,0.186916384615149,0.249220212785669,0.31152404095619,
0.37382786912671,0.436134147349024,0.498440425571339,0.560746703793653,
0.623052982015967,0.685356810186488,0.747660638357008),.UNSPECIFIED.);
#267=B_SPLINE_CURVE_WITH_KNOTS('',3,(#10028,#10029,#10030,#10031,#10032,
#10033,#10034,#10035,#10036,#10037),.UNSPECIFIED.,.F.,.F.,(4,2,2,2,4),(0.747660638357008,
0.809964466527528,0.872268294698049,0.934574572920363,0.996880851142677),
 .UNSPECIFIED.);
#268=B_SPLINE_CURVE_WITH_KNOTS('',3,(#10038,#10039,#10040,#10041,#10042,
#10043,#10044,#10045),.UNSPECIFIED.,.F.,.F.,(4,2,2,4),(0.117322411671485,
0.125333990377958,0.187974273370181,0.250614556362404),.UNSPECIFIED.);
#269=B_SPLINE_CURVE_WITH_KNOTS('',3,(#10460,#10461,#10462,#10463,#10464,
#10465,#10466,#10467,#10468,#10469,#10470,#10471,#10472,#10473,#10474,#10475,
#10476,#10477,#10478,#10479,#10480,#10481),.UNSPECIFIED.,.F.,.F.,(4,2,2,
2,2,2,2,2,2,2,4),(0.0473477652366656,0.126350602536658,0.189525903804987,
0.252701205073317,0.313298422430275,0.373895639787233,0.434492857144191,
0.495090074501149,0.558265375769478,0.621440677037807,0.7004435143378),
 .UNSPECIFIED.);
#270=B_SPLINE_CURVE_WITH_KNOTS('',3,(#10485,#10486,#10487,#10488,#10489,
#10490,#10491,#10492,#10493,#10494,#10495,#10496,#10497,#10498,#10499,#10500,
#10501,#10502,#10503,#10504,#10505,#10506),.UNSPECIFIED.,.F.,.F.,(4,2,2,
2,2,2,2,2,2,2,4),(0.0464897534940957,0.0852567806515119,0.170513561303024,
0.246687263103517,0.308657850341199,0.370628437578881,0.432599024816563,
0.494569612054245,0.570743313854739,0.656000094506251,0.694767121663666),
 .UNSPECIFIED.);
#271=B_SPLINE_CURVE_WITH_KNOTS('',3,(#10512,#10513,#10514,#10515,#10516,
#10517,#10518,#10519,#10520,#10521,#10522,#10523,#10524,#10525,#10526,#10527,
#10528,#10529,#10530,#10531,#10532,#10533),.UNSPECIFIED.,.F.,.F.,(4,2,2,
2,2,2,2,2,2,2,4),(0.0464897534940957,0.0852567806515118,0.170513561303024,
0.246687263103517,0.308657850341199,0.370628437578881,0.432599024816563,
0.494569612054245,0.570743313854738,0.65600009450625,0.694767121663666),
 .UNSPECIFIED.);
#272=B_SPLINE_CURVE_WITH_KNOTS('',3,(#10537,#10538,#10539,#10540,#10541,
#10542,#10543,#10544,#10545,#10546,#10547,#10548,#10549,#10550,#10551,#10552,
#10553,#10554,#10555,#10556,#10557,#10558),.UNSPECIFIED.,.F.,.F.,(4,2,2,
2,2,2,2,2,2,2,4),(0.0464897534940957,0.0852567806515119,0.170513561303024,
0.246687263103517,0.308657850341199,0.370628437578881,0.432599024816563,
0.494569612054245,0.570743313854739,0.656000094506251,0.694767121663666),
 .UNSPECIFIED.);
#273=B_SPLINE_CURVE_WITH_KNOTS('',3,(#10562,#10563,#10564,#10565,#10566,
#10567,#10568,#10569,#10570,#10571,#10572,#10573),.UNSPECIFIED.,.F.,.F.,
(4,2,2,2,2,4),(0.0464897534940957,0.0852567806515119,0.170513561303024,
0.246687263103517,0.308657850341199,0.370628437578881),.UNSPECIFIED.);
#274=B_SPLINE_CURVE_WITH_KNOTS('',3,(#10578,#10579,#10580,#10581,#10582,
#10583,#10584,#10585,#10586,#10587,#10588,#10589),.UNSPECIFIED.,.F.,.F.,
(4,2,2,2,2,4),(0.370628437578881,0.432599024816563,0.494569612054245,0.570743313854738,
0.65600009450625,0.694767121663666),.UNSPECIFIED.);
#275=B_SPLINE_CURVE_WITH_KNOTS('',3,(#10593,#10594,#10595,#10596,#10597,
#10598,#10599,#10600,#10601,#10602,#10603,#10604,#10605,#10606,#10607,#10608,
#10609,#10610,#10611,#10612,#10613,#10614),.UNSPECIFIED.,.F.,.F.,(4,2,2,
2,2,2,2,2,2,2,4),(0.0464897534940957,0.0852567806515121,0.170513561303024,
0.246687263103518,0.308657850341199,0.370628437578881,0.432599024816563,
0.494569612054245,0.570743313854738,0.65600009450625,0.694767121663666),
 .UNSPECIFIED.);
#276=B_SPLINE_CURVE_WITH_KNOTS('',3,(#10618,#10619,#10620,#10621,#10622,
#10623,#10624,#10625,#10626,#10627,#10628,#10629,#10630,#10631,#10632,#10633,
#10634,#10635,#10636,#10637,#10638,#10639),.UNSPECIFIED.,.F.,.F.,(4,2,2,
2,2,2,2,2,2,2,4),(0.0464897534940957,0.0852567806515119,0.170513561303024,
0.246687263103517,0.308657850341199,0.370628437578881,0.432599024816563,
0.494569612054245,0.570743313854738,0.65600009450625,0.694767121663667),
 .UNSPECIFIED.);
#277=B_SPLINE_CURVE_WITH_KNOTS('',3,(#10643,#10644,#10645,#10646,#10647,
#10648,#10649,#10650,#10651,#10652,#10653,#10654,#10655,#10656,#10657,#10658,
#10659,#10660,#10661,#10662,#10663,#10664),.UNSPECIFIED.,.F.,.F.,(4,2,2,
2,2,2,2,2,2,2,4),(0.0464897534940957,0.0852567806515119,0.170513561303024,
0.246687263103517,0.308657850341199,0.370628437578881,0.432599024816563,
0.494569612054245,0.570743313854738,0.65600009450625,0.694767121663666),
 .UNSPECIFIED.);
#278=B_SPLINE_CURVE_WITH_KNOTS('',3,(#10668,#10669,#10670,#10671,#10672,
#10673,#10674,#10675,#10676,#10677,#10678,#10679,#10680,#10681,#10682,#10683,
#10684,#10685,#10686,#10687,#10688,#10689),.UNSPECIFIED.,.F.,.F.,(4,2,2,
2,2,2,2,2,2,2,4),(0.0464897534940957,0.0852567806515119,0.170513561303024,
0.246687263103517,0.308657850341199,0.370628437578881,0.432599024816563,
0.494569612054245,0.570743313854739,0.656000094506251,0.694767121663667),
 .UNSPECIFIED.);
#279=B_SPLINE_CURVE_WITH_KNOTS('',3,(#10697,#10698,#10699,#10700,#10701,
#10702,#10703,#10704,#10705,#10706,#10707,#10708,#10709,#10710,#10711,#10712,
#10713,#10714,#10715,#10716,#10717,#10718),.UNSPECIFIED.,.F.,.F.,(4,2,2,
2,2,2,2,2,2,2,4),(0.0473477652366656,0.126350602536658,0.189525903804987,
0.252701205073316,0.313298422430274,0.373895639787232,0.434492857144191,
0.495090074501149,0.558265375769478,0.621440677037807,0.7004435143378),
 .UNSPECIFIED.);
#280=B_SPLINE_CURVE_WITH_KNOTS('',3,(#10726,#10727,#10728,#10729,#10730,
#10731,#10732,#10733,#10734,#10735,#10736,#10737,#10738,#10739,#10740,#10741,
#10742,#10743,#10744,#10745,#10746,#10747),.UNSPECIFIED.,.F.,.F.,(4,2,2,
2,2,2,2,2,2,2,4),(0.0473477652366656,0.126350602536658,0.189525903804987,
0.252701205073317,0.313298422430275,0.373895639787233,0.434492857144191,
0.495090074501149,0.558265375769478,0.621440677037807,0.7004435143378),
 .UNSPECIFIED.);
#281=B_SPLINE_CURVE_WITH_KNOTS('',3,(#10756,#10757,#10758,#10759,#10760,
#10761,#10762,#10763,#10764,#10765,#10766,#10767),.UNSPECIFIED.,.F.,.F.,
(4,2,2,2,2,4),(0.0473477652366656,0.126350602536658,0.189525903804987,0.252701205073316,
0.313298422430275,0.373895639787233),.UNSPECIFIED.);
#282=B_SPLINE_CURVE_WITH_KNOTS('',3,(#10769,#10770,#10771,#10772,#10773,
#10774,#10775,#10776,#10777,#10778,#10779,#10780),.UNSPECIFIED.,.F.,.F.,
(4,2,2,2,2,4),(0.373895639787233,0.434492857144191,0.495090074501149,0.558265375769478,
0.621440677037807,0.7004435143378),.UNSPECIFIED.);
#283=B_SPLINE_CURVE_WITH_KNOTS('',3,(#10787,#10788,#10789,#10790,#10791,
#10792,#10793,#10794,#10795,#10796,#10797,#10798,#10799,#10800,#10801,#10802,
#10803,#10804,#10805,#10806,#10807,#10808),.UNSPECIFIED.,.F.,.F.,(4,2,2,
2,2,2,2,2,2,2,4),(0.0473477652366656,0.126350602536658,0.189525903804987,
0.252701205073316,0.313298422430275,0.373895639787233,0.434492857144191,
0.495090074501149,0.558265375769478,0.621440677037807,0.7004435143378),
 .UNSPECIFIED.);
#284=B_SPLINE_CURVE_WITH_KNOTS('',3,(#10816,#10817,#10818,#10819,#10820,
#10821,#10822,#10823,#10824,#10825,#10826,#10827,#10828,#10829,#10830,#10831,
#10832,#10833,#10834,#10835,#10836,#10837),.UNSPECIFIED.,.F.,.F.,(4,2,2,
2,2,2,2,2,2,2,4),(0.0473477652366656,0.126350602536658,0.189525903804987,
0.252701205073317,0.313298422430275,0.373895639787233,0.434492857144191,
0.495090074501149,0.558265375769478,0.621440677037807,0.7004435143378),
 .UNSPECIFIED.);
#285=B_SPLINE_CURVE_WITH_KNOTS('',3,(#10845,#10846,#10847,#10848,#10849,
#10850,#10851,#10852,#10853,#10854,#10855,#10856,#10857,#10858,#10859,#10860,
#10861,#10862,#10863,#10864,#10865,#10866),.UNSPECIFIED.,.F.,.F.,(4,2,2,
2,2,2,2,2,2,2,4),(0.0473477652366656,0.126350602536658,0.189525903804987,
0.252701205073316,0.313298422430275,0.373895639787233,0.434492857144191,
0.495090074501149,0.558265375769478,0.621440677037807,0.7004435143378),
 .UNSPECIFIED.);
#286=B_SPLINE_CURVE_WITH_KNOTS('',3,(#10875,#10876,#10877,#10878,#10879,
#10880,#10881,#10882,#10883,#10884,#10885,#10886,#10887,#10888,#10889,#10890,
#10891,#10892,#10893,#10894,#10895,#10896),.UNSPECIFIED.,.F.,.F.,(4,2,2,
2,2,2,2,2,2,2,4),(0.0473477652366656,0.126350602536658,0.189525903804987,
0.252701205073317,0.313298422430275,0.373895639787233,0.434492857144191,
0.495090074501149,0.558265375769478,0.621440677037807,0.7004435143378),
 .UNSPECIFIED.);
#287=SHAPE_REPRESENTATION_RELATIONSHIP('SRR','None',#11155,#312);
#288=SHAPE_REPRESENTATION_RELATIONSHIP('SRR','None',#11156,#313);
#289=SHAPE_REPRESENTATION_RELATIONSHIP('SRR','None',#11157,#314);
#290=SHAPE_REPRESENTATION_RELATIONSHIP('SRR','None',#11158,#315);
#291=SHAPE_REPRESENTATION_RELATIONSHIP('SRR','None',#11159,#316);
#292=SHAPE_REPRESENTATION_RELATIONSHIP('SRR','None',#11160,#317);
#293=SHAPE_REPRESENTATION_RELATIONSHIP('SRR','None',#11161,#318);
#294=SHAPE_REPRESENTATION_RELATIONSHIP('SRR','None',#11163,#319);
#295=SHAPE_REPRESENTATION_RELATIONSHIP('SRR','None',#11164,#320);
#296=SHAPE_REPRESENTATION_RELATIONSHIP('SRR','None',#11165,#321);
#297=SHAPE_REPRESENTATION_RELATIONSHIP('SRR','None',#11167,#322);
#298=SHAPE_REPRESENTATION_RELATIONSHIP('SRR','None',#11168,#323);
#299=SHAPE_REPRESENTATION_RELATIONSHIP('SRR','None',#11169,#324);
#300=SHAPE_REPRESENTATION_RELATIONSHIP('SRR','None',#11170,#325);
#301=SHAPE_REPRESENTATION_RELATIONSHIP('SRR','None',#11172,#326);
#302=SHAPE_REPRESENTATION_RELATIONSHIP('SRR','None',#11173,#327);
#303=SHAPE_REPRESENTATION_RELATIONSHIP('SRR','None',#11174,#328);
#304=SHAPE_REPRESENTATION_RELATIONSHIP('SRR','None',#11175,#329);
#305=SHAPE_REPRESENTATION_RELATIONSHIP('SRR','None',#11176,#330);
#306=SHAPE_REPRESENTATION_RELATIONSHIP('SRR','None',#11177,#331);
#307=SHAPE_REPRESENTATION_RELATIONSHIP('SRR','None',#11180,#332);
#308=SHAPE_REPRESENTATION_RELATIONSHIP('SRR','None',#11181,#333);
#309=SHAPE_REPRESENTATION_RELATIONSHIP('SRR','None',#11182,#334);
#310=SHAPE_REPRESENTATION_RELATIONSHIP('SRR','None',#11183,#335);
#311=SHAPE_REPRESENTATION_RELATIONSHIP('SRR','None',#11184,#336);
#312=ADVANCED_BREP_SHAPE_REPRESENTATION('',(#370),#11005);
#313=ADVANCED_BREP_SHAPE_REPRESENTATION('',(#371),#11006);
#314=ADVANCED_BREP_SHAPE_REPRESENTATION('',(#372),#11007);
#315=ADVANCED_BREP_SHAPE_REPRESENTATION('',(#373),#11008);
#316=ADVANCED_BREP_SHAPE_REPRESENTATION('',(#374),#11009);
#317=ADVANCED_BREP_SHAPE_REPRESENTATION('',(#375),#11010);
#318=ADVANCED_BREP_SHAPE_REPRESENTATION('',(#376),#11011);
#319=ADVANCED_BREP_SHAPE_REPRESENTATION('',(#377),#11013);
#320=ADVANCED_BREP_SHAPE_REPRESENTATION('',(#378),#11014);
#321=ADVANCED_BREP_SHAPE_REPRESENTATION('',(#42),#11015);
#322=ADVANCED_BREP_SHAPE_REPRESENTATION('',(#379),#11017);
#323=ADVANCED_BREP_SHAPE_REPRESENTATION('',(#380),#11018);
#324=ADVANCED_BREP_SHAPE_REPRESENTATION('',(#381),#11019);
#325=ADVANCED_BREP_SHAPE_REPRESENTATION('',(#382),#11020);
#326=ADVANCED_BREP_SHAPE_REPRESENTATION('',(#383),#11022);
#327=ADVANCED_BREP_SHAPE_REPRESENTATION('',(#384),#11023);
#328=ADVANCED_BREP_SHAPE_REPRESENTATION('',(#385),#11024);
#329=ADVANCED_BREP_SHAPE_REPRESENTATION('',(#386),#11025);
#330=ADVANCED_BREP_SHAPE_REPRESENTATION('',(#387),#11026);
#331=ADVANCED_BREP_SHAPE_REPRESENTATION('',(#43),#11027);
#332=ADVANCED_BREP_SHAPE_REPRESENTATION('',(#388),#11030);
#333=ADVANCED_BREP_SHAPE_REPRESENTATION('',(#389),#11031);
#334=ADVANCED_BREP_SHAPE_REPRESENTATION('',(#390,#391,#392,#393,#394,#395,
#396,#397),#11032);
#335=ADVANCED_BREP_SHAPE_REPRESENTATION('',(#398),#11033);
#336=ADVANCED_BREP_SHAPE_REPRESENTATION('',(#399,#400),#11034);
#337=STYLED_ITEM('',(#11365),#370);
#338=STYLED_ITEM('',(#11400),#371);
#339=STYLED_ITEM('',(#11379),#372);
#340=STYLED_ITEM('',(#11379),#373);
#341=STYLED_ITEM('',(#11386),#374);
#342=STYLED_ITEM('',(#11400),#375);
#343=STYLED_ITEM('',(#11372),#376);
#344=STYLED_ITEM('',(#11400),#377);
#345=STYLED_ITEM('',(#11379),#378);
#346=STYLED_ITEM('',(#11393),#42);
#347=STYLED_ITEM('',(#11379),#379);
#348=STYLED_ITEM('',(#11372),#380);
#349=STYLED_ITEM('',(#11379),#381);
#350=STYLED_ITEM('',(#11393),#382);
#351=STYLED_ITEM('',(#11400),#383);
#352=STYLED_ITEM('',(#11386),#384);
#353=STYLED_ITEM('',(#11379),#385);
#354=STYLED_ITEM('',(#11379),#386);
#355=STYLED_ITEM('',(#11386),#387);
#356=STYLED_ITEM('',(#11393),#43);
#357=STYLED_ITEM('',(#11386),#388);
#358=STYLED_ITEM('',(#11386),#389);
#359=STYLED_ITEM('',(#11386),#390);
#360=STYLED_ITEM('',(#11386),#391);
#361=STYLED_ITEM('',(#11386),#392);
#362=STYLED_ITEM('',(#11386),#393);
#363=STYLED_ITEM('',(#11386),#394);
#364=STYLED_ITEM('',(#11386),#395);
#365=STYLED_ITEM('',(#11386),#396);
#366=STYLED_ITEM('',(#11386),#397);
#367=STYLED_ITEM('',(#11386),#398);
#368=STYLED_ITEM('',(#11386),#399);
#369=STYLED_ITEM('',(#11386),#400);
#370=MANIFOLD_SOLID_BREP('Body1',#4705);
#371=MANIFOLD_SOLID_BREP('Body1',#4706);
#372=MANIFOLD_SOLID_BREP('Body1',#4707);
#373=MANIFOLD_SOLID_BREP('Body1',#4708);
#374=MANIFOLD_SOLID_BREP('Body1',#4709);
#375=MANIFOLD_SOLID_BREP('Body1',#4710);
#376=MANIFOLD_SOLID_BREP('Body1',#4711);
#377=MANIFOLD_SOLID_BREP('Body1',#4712);
#378=MANIFOLD_SOLID_BREP('Body1',#4713);
#379=MANIFOLD_SOLID_BREP('Body1',#4716);
#380=MANIFOLD_SOLID_BREP('Body1',#4717);
#381=MANIFOLD_SOLID_BREP('Body1',#4718);
#382=MANIFOLD_SOLID_BREP('Body1',#4719);
#383=MANIFOLD_SOLID_BREP('Body1',#4720);
#384=MANIFOLD_SOLID_BREP('Body1',#4721);
#385=MANIFOLD_SOLID_BREP('Body1',#4722);
#386=MANIFOLD_SOLID_BREP('Body1',#4723);
#387=MANIFOLD_SOLID_BREP('Body1',#4724);
#388=MANIFOLD_SOLID_BREP('Body1',#4727);
#389=MANIFOLD_SOLID_BREP('Body1',#4728);
#390=MANIFOLD_SOLID_BREP('Body1',#4729);
#391=MANIFOLD_SOLID_BREP('Body2',#4730);
#392=MANIFOLD_SOLID_BREP('Body3',#4731);
#393=MANIFOLD_SOLID_BREP('Body4',#4732);
#394=MANIFOLD_SOLID_BREP('Body5',#4733);
#395=MANIFOLD_SOLID_BREP('Body6',#4734);
#396=MANIFOLD_SOLID_BREP('Body7',#4735);
#397=MANIFOLD_SOLID_BREP('Body8',#4736);
#398=MANIFOLD_SOLID_BREP('Continuous crown cage',#4737);
#399=MANIFOLD_SOLID_BREP('Body1',#4738);
#400=MANIFOLD_SOLID_BREP('Body2',#4739);
#401=FACE_BOUND('',#951,.T.);
#402=FACE_BOUND('',#952,.T.);
#403=FACE_BOUND('',#953,.T.);
#404=FACE_BOUND('',#954,.T.);
#405=FACE_BOUND('',#955,.T.);
#406=FACE_BOUND('',#956,.T.);
#407=FACE_BOUND('',#958,.T.);
#408=FACE_BOUND('',#959,.T.);
#409=FACE_BOUND('',#960,.T.);
#410=FACE_BOUND('',#961,.T.);
#411=FACE_BOUND('',#962,.T.);
#412=FACE_BOUND('',#963,.T.);
#413=FACE_BOUND('',#965,.T.);
#414=FACE_BOUND('',#966,.T.);
#415=FACE_BOUND('',#978,.T.);
#416=FACE_BOUND('',#979,.T.);
#417=FACE_BOUND('',#980,.T.);
#418=FACE_BOUND('',#981,.T.);
#419=FACE_BOUND('',#982,.T.);
#420=FACE_BOUND('',#984,.T.);
#421=FACE_BOUND('',#987,.T.);
#422=FACE_BOUND('',#988,.T.);
#423=FACE_BOUND('',#989,.T.);
#424=FACE_BOUND('',#990,.T.);
#425=FACE_BOUND('',#991,.T.);
#426=FACE_BOUND('',#993,.T.);
#427=FACE_BOUND('',#996,.T.);
#428=FACE_BOUND('',#997,.T.);
#429=FACE_BOUND('',#999,.T.);
#430=FACE_BOUND('',#1000,.T.);
#431=FACE_BOUND('',#1001,.T.);
#432=FACE_BOUND('',#1002,.T.);
#433=FACE_BOUND('',#1003,.T.);
#434=FACE_BOUND('',#1005,.T.);
#435=FACE_BOUND('',#1006,.T.);
#436=FACE_BOUND('',#1007,.T.);
#437=FACE_BOUND('',#1008,.T.);
#438=FACE_BOUND('',#1009,.T.);
#439=FACE_BOUND('',#1011,.T.);
#440=FACE_BOUND('',#1012,.T.);
#441=FACE_BOUND('',#1018,.T.);
#442=FACE_BOUND('',#1025,.T.);
#443=FACE_BOUND('',#1031,.T.);
#444=FACE_BOUND('',#1038,.T.);
#445=FACE_BOUND('',#1061,.T.);
#446=FACE_BOUND('',#1062,.T.);
#447=FACE_BOUND('',#1063,.T.);
#448=FACE_BOUND('',#1064,.T.);
#449=FACE_BOUND('',#1065,.T.);
#450=FACE_BOUND('',#1072,.T.);
#451=FACE_BOUND('',#1074,.T.);
#452=FACE_BOUND('',#1076,.T.);
#453=FACE_BOUND('',#1078,.T.);
#454=FACE_BOUND('',#1079,.T.);
#455=FACE_BOUND('',#1080,.T.);
#456=FACE_BOUND('',#1081,.T.);
#457=FACE_BOUND('',#1082,.T.);
#458=FACE_BOUND('',#1084,.T.);
#459=FACE_BOUND('',#1085,.T.);
#460=FACE_BOUND('',#1086,.T.);
#461=FACE_BOUND('',#1087,.T.);
#462=FACE_BOUND('',#1088,.T.);
#463=FACE_BOUND('',#1091,.T.);
#464=FACE_BOUND('',#1094,.T.);
#465=FACE_BOUND('',#1097,.T.);
#466=FACE_BOUND('',#1100,.T.);
#467=FACE_BOUND('',#1107,.T.);
#468=FACE_BOUND('',#1111,.T.);
#469=FACE_BOUND('',#1112,.T.);
#470=FACE_BOUND('',#1113,.T.);
#471=FACE_BOUND('',#1114,.T.);
#472=FACE_BOUND('',#1115,.T.);
#473=FACE_BOUND('',#1117,.T.);
#474=FACE_BOUND('',#1118,.T.);
#475=FACE_BOUND('',#1119,.T.);
#476=FACE_BOUND('',#1120,.T.);
#477=FACE_BOUND('',#1121,.T.);
#478=FACE_BOUND('',#1128,.T.);
#479=FACE_BOUND('',#1131,.T.);
#480=FACE_BOUND('',#1134,.T.);
#481=FACE_BOUND('',#1137,.T.);
#482=FACE_BOUND('',#1140,.T.);
#483=FACE_BOUND('',#1143,.T.);
#484=FACE_BOUND('',#1145,.T.);
#485=FACE_BOUND('',#1151,.T.);
#486=FACE_BOUND('',#1153,.T.);
#487=FACE_BOUND('',#1155,.T.);
#488=FACE_BOUND('',#1157,.T.);
#489=FACE_BOUND('',#1172,.T.);
#490=FACE_BOUND('',#1176,.T.);
#491=FACE_BOUND('',#1178,.T.);
#492=FACE_BOUND('',#1181,.T.);
#493=FACE_BOUND('',#1190,.T.);
#494=FACE_BOUND('',#1192,.T.);
#495=FACE_BOUND('',#1197,.T.);
#496=FACE_BOUND('',#1199,.T.);
#497=FACE_BOUND('',#1201,.T.);
#498=FACE_BOUND('',#1203,.T.);
#499=FACE_BOUND('',#1213,.T.);
#500=FACE_BOUND('',#1221,.T.);
#501=FACE_BOUND('',#1227,.T.);
#502=FACE_BOUND('',#1229,.T.);
#503=FACE_BOUND('',#1233,.T.);
#504=FACE_BOUND('',#1235,.T.);
#505=FACE_BOUND('',#1242,.T.);
#506=FACE_BOUND('',#1247,.T.);
#507=FACE_BOUND('',#1251,.T.);
#508=FACE_BOUND('',#1253,.T.);
#509=FACE_BOUND('',#1257,.T.);
#510=FACE_BOUND('',#1259,.T.);
#511=FACE_BOUND('',#1263,.T.);
#512=FACE_BOUND('',#1265,.T.);
#513=FACE_BOUND('',#1280,.T.);
#514=FACE_BOUND('',#1288,.T.);
#515=FACE_BOUND('',#1291,.T.);
#516=FACE_BOUND('',#1296,.T.);
#517=FACE_BOUND('',#1301,.T.);
#518=FACE_BOUND('',#1329,.T.);
#519=FACE_BOUND('',#1332,.T.);
#520=FACE_BOUND('',#1335,.T.);
#521=FACE_BOUND('',#1338,.T.);
#522=FACE_BOUND('',#1341,.T.);
#523=PLANE('',#5037);
#524=PLANE('',#5038);
#525=PLANE('',#5039);
#526=PLANE('',#5040);
#527=PLANE('',#5041);
#528=PLANE('',#5042);
#529=PLANE('',#5044);
#530=PLANE('',#5047);
#531=PLANE('',#5048);
#532=PLANE('',#5067);
#533=PLANE('',#5073);
#534=PLANE('',#5080);
#535=PLANE('',#5081);
#536=PLANE('',#5082);
#537=PLANE('',#5096);
#538=PLANE('',#5112);
#539=PLANE('',#5126);
#540=PLANE('',#5142);
#541=PLANE('',#5146);
#542=PLANE('',#5147);
#543=PLANE('',#5153);
#544=PLANE('',#5157);
#545=PLANE('',#5161);
#546=PLANE('',#5165);
#547=PLANE('',#5166);
#548=PLANE('',#5174);
#549=PLANE('',#5179);
#550=PLANE('',#5184);
#551=PLANE('',#5193);
#552=PLANE('',#5210);
#553=PLANE('',#5216);
#554=PLANE('',#5217);
#555=PLANE('',#5222);
#556=PLANE('',#5227);
#557=PLANE('',#5232);
#558=PLANE('',#5237);
#559=PLANE('',#5250);
#560=PLANE('',#5257);
#561=PLANE('',#5258);
#562=PLANE('',#5261);
#563=PLANE('',#5263);
#564=PLANE('',#5264);
#565=PLANE('',#5266);
#566=PLANE('',#5267);
#567=PLANE('',#5268);
#568=PLANE('',#5273);
#569=PLANE('',#5277);
#570=PLANE('',#5281);
#571=PLANE('',#5285);
#572=PLANE('',#5289);
#573=PLANE('',#5293);
#574=PLANE('',#5296);
#575=PLANE('',#5297);
#576=PLANE('',#5300);
#577=PLANE('',#5301);
#578=PLANE('',#5306);
#579=PLANE('',#5312);
#580=PLANE('',#5313);
#581=PLANE('',#5314);
#582=PLANE('',#5315);
#583=PLANE('',#5316);
#584=PLANE('',#5317);
#585=PLANE('',#5318);
#586=PLANE('',#5319);
#587=PLANE('',#5320);
#588=PLANE('',#5322);
#589=PLANE('',#5330);
#590=PLANE('',#5337);
#591=PLANE('',#5340);
#592=PLANE('',#5344);
#593=PLANE('',#5352);
#594=PLANE('',#5353);
#595=PLANE('',#5361);
#596=PLANE('',#5362);
#597=PLANE('',#5364);
#598=PLANE('',#5368);
#599=PLANE('',#5375);
#600=PLANE('',#5376);
#601=PLANE('',#5378);
#602=PLANE('',#5380);
#603=PLANE('',#5381);
#604=PLANE('',#5382);
#605=PLANE('',#5383);
#606=PLANE('',#5384);
#607=PLANE('',#5385);
#608=PLANE('',#5386);
#609=PLANE('',#5387);
#610=PLANE('',#5398);
#611=PLANE('',#5400);
#612=PLANE('',#5406);
#613=PLANE('',#5408);
#614=PLANE('',#5418);
#615=PLANE('',#5419);
#616=PLANE('',#5420);
#617=PLANE('',#5424);
#618=PLANE('',#5425);
#619=PLANE('',#5428);
#620=PLANE('',#5429);
#621=PLANE('',#5434);
#622=PLANE('',#5435);
#623=PLANE('',#5440);
#624=PLANE('',#5443);
#625=PLANE('',#5451);
#626=PLANE('',#5452);
#627=PLANE('',#5460);
#628=PLANE('',#5461);
#629=PLANE('',#5469);
#630=PLANE('',#5470);
#631=PLANE('',#5472);
#632=PLANE('',#5473);
#633=PLANE('',#5474);
#634=PLANE('',#5475);
#635=PLANE('',#5476);
#636=PLANE('',#5477);
#637=PLANE('',#5478);
#638=PLANE('',#5479);
#639=PLANE('',#5480);
#640=PLANE('',#5482);
#641=PLANE('',#5490);
#642=PLANE('',#5517);
#643=PLANE('',#5520);
#644=PLANE('',#5532);
#645=PLANE('',#5541);
#646=PLANE('',#5574);
#647=PLANE('',#5579);
#648=PLANE('',#5584);
#649=PLANE('',#5589);
#650=PLANE('',#5594);
#651=PLANE('',#5599);
#652=PLANE('',#5608);
#653=PLANE('',#5612);
#654=PLANE('',#5613);
#655=PLANE('',#5615);
#656=PLANE('',#5620);
#657=PLANE('',#5623);
#658=PLANE('',#5628);
#659=FACE_OUTER_BOUND('',#940,.T.);
#660=FACE_OUTER_BOUND('',#941,.T.);
#661=FACE_OUTER_BOUND('',#942,.T.);
#662=FACE_OUTER_BOUND('',#943,.T.);
#663=FACE_OUTER_BOUND('',#944,.T.);
#664=FACE_OUTER_BOUND('',#945,.T.);
#665=FACE_OUTER_BOUND('',#946,.T.);
#666=FACE_OUTER_BOUND('',#947,.T.);
#667=FACE_OUTER_BOUND('',#948,.T.);
#668=FACE_OUTER_BOUND('',#949,.T.);
#669=FACE_OUTER_BOUND('',#950,.T.);
#670=FACE_OUTER_BOUND('',#957,.T.);
#671=FACE_OUTER_BOUND('',#964,.T.);
#672=FACE_OUTER_BOUND('',#967,.T.);
#673=FACE_OUTER_BOUND('',#968,.T.);
#674=FACE_OUTER_BOUND('',#969,.T.);
#675=FACE_OUTER_BOUND('',#970,.T.);
#676=FACE_OUTER_BOUND('',#971,.T.);
#677=FACE_OUTER_BOUND('',#972,.T.);
#678=FACE_OUTER_BOUND('',#973,.T.);
#679=FACE_OUTER_BOUND('',#974,.T.);
#680=FACE_OUTER_BOUND('',#975,.T.);
#681=FACE_OUTER_BOUND('',#976,.T.);
#682=FACE_OUTER_BOUND('',#977,.T.);
#683=FACE_OUTER_BOUND('',#983,.T.);
#684=FACE_OUTER_BOUND('',#985,.T.);
#685=FACE_OUTER_BOUND('',#986,.T.);
#686=FACE_OUTER_BOUND('',#992,.T.);
#687=FACE_OUTER_BOUND('',#994,.T.);
#688=FACE_OUTER_BOUND('',#995,.T.);
#689=FACE_OUTER_BOUND('',#998,.T.);
#690=FACE_OUTER_BOUND('',#1004,.T.);
#691=FACE_OUTER_BOUND('',#1010,.T.);
#692=FACE_OUTER_BOUND('',#1013,.T.);
#693=FACE_OUTER_BOUND('',#1014,.T.);
#694=FACE_OUTER_BOUND('',#1015,.T.);
#695=FACE_OUTER_BOUND('',#1016,.T.);
#696=FACE_OUTER_BOUND('',#1017,.T.);
#697=FACE_OUTER_BOUND('',#1019,.T.);
#698=FACE_OUTER_BOUND('',#1020,.T.);
#699=FACE_OUTER_BOUND('',#1021,.T.);
#700=FACE_OUTER_BOUND('',#1022,.T.);
#701=FACE_OUTER_BOUND('',#1023,.T.);
#702=FACE_OUTER_BOUND('',#1024,.T.);
#703=FACE_OUTER_BOUND('',#1026,.T.);
#704=FACE_OUTER_BOUND('',#1027,.T.);
#705=FACE_OUTER_BOUND('',#1028,.T.);
#706=FACE_OUTER_BOUND('',#1029,.T.);
#707=FACE_OUTER_BOUND('',#1030,.T.);
#708=FACE_OUTER_BOUND('',#1032,.T.);
#709=FACE_OUTER_BOUND('',#1033,.T.);
#710=FACE_OUTER_BOUND('',#1034,.T.);
#711=FACE_OUTER_BOUND('',#1035,.T.);
#712=FACE_OUTER_BOUND('',#1036,.T.);
#713=FACE_OUTER_BOUND('',#1037,.T.);
#714=FACE_OUTER_BOUND('',#1039,.T.);
#715=FACE_OUTER_BOUND('',#1040,.T.);
#716=FACE_OUTER_BOUND('',#1041,.T.);
#717=FACE_OUTER_BOUND('',#1042,.T.);
#718=FACE_OUTER_BOUND('',#1043,.T.);
#719=FACE_OUTER_BOUND('',#1044,.T.);
#720=FACE_OUTER_BOUND('',#1045,.T.);
#721=FACE_OUTER_BOUND('',#1046,.T.);
#722=FACE_OUTER_BOUND('',#1047,.T.);
#723=FACE_OUTER_BOUND('',#1048,.T.);
#724=FACE_OUTER_BOUND('',#1049,.T.);
#725=FACE_OUTER_BOUND('',#1050,.T.);
#726=FACE_OUTER_BOUND('',#1051,.T.);
#727=FACE_OUTER_BOUND('',#1052,.T.);
#728=FACE_OUTER_BOUND('',#1053,.T.);
#729=FACE_OUTER_BOUND('',#1054,.T.);
#730=FACE_OUTER_BOUND('',#1055,.T.);
#731=FACE_OUTER_BOUND('',#1056,.T.);
#732=FACE_OUTER_BOUND('',#1057,.T.);
#733=FACE_OUTER_BOUND('',#1058,.T.);
#734=FACE_OUTER_BOUND('',#1059,.T.);
#735=FACE_OUTER_BOUND('',#1060,.T.);
#736=FACE_OUTER_BOUND('',#1066,.T.);
#737=FACE_OUTER_BOUND('',#1067,.T.);
#738=FACE_OUTER_BOUND('',#1068,.T.);
#739=FACE_OUTER_BOUND('',#1069,.T.);
#740=FACE_OUTER_BOUND('',#1070,.T.);
#741=FACE_OUTER_BOUND('',#1071,.T.);
#742=FACE_OUTER_BOUND('',#1073,.T.);
#743=FACE_OUTER_BOUND('',#1075,.T.);
#744=FACE_OUTER_BOUND('',#1077,.T.);
#745=FACE_OUTER_BOUND('',#1083,.T.);
#746=FACE_OUTER_BOUND('',#1089,.T.);
#747=FACE_OUTER_BOUND('',#1090,.T.);
#748=FACE_OUTER_BOUND('',#1092,.T.);
#749=FACE_OUTER_BOUND('',#1093,.T.);
#750=FACE_OUTER_BOUND('',#1095,.T.);
#751=FACE_OUTER_BOUND('',#1096,.T.);
#752=FACE_OUTER_BOUND('',#1098,.T.);
#753=FACE_OUTER_BOUND('',#1099,.T.);
#754=FACE_OUTER_BOUND('',#1101,.T.);
#755=FACE_OUTER_BOUND('',#1102,.T.);
#756=FACE_OUTER_BOUND('',#1103,.T.);
#757=FACE_OUTER_BOUND('',#1104,.T.);
#758=FACE_OUTER_BOUND('',#1105,.T.);
#759=FACE_OUTER_BOUND('',#1106,.T.);
#760=FACE_OUTER_BOUND('',#1108,.T.);
#761=FACE_OUTER_BOUND('',#1109,.T.);
#762=FACE_OUTER_BOUND('',#1110,.T.);
#763=FACE_OUTER_BOUND('',#1116,.T.);
#764=FACE_OUTER_BOUND('',#1122,.T.);
#765=FACE_OUTER_BOUND('',#1123,.T.);
#766=FACE_OUTER_BOUND('',#1124,.T.);
#767=FACE_OUTER_BOUND('',#1125,.T.);
#768=FACE_OUTER_BOUND('',#1126,.T.);
#769=FACE_OUTER_BOUND('',#1127,.T.);
#770=FACE_OUTER_BOUND('',#1129,.T.);
#771=FACE_OUTER_BOUND('',#1130,.T.);
#772=FACE_OUTER_BOUND('',#1132,.T.);
#773=FACE_OUTER_BOUND('',#1133,.T.);
#774=FACE_OUTER_BOUND('',#1135,.T.);
#775=FACE_OUTER_BOUND('',#1136,.T.);
#776=FACE_OUTER_BOUND('',#1138,.T.);
#777=FACE_OUTER_BOUND('',#1139,.T.);
#778=FACE_OUTER_BOUND('',#1141,.T.);
#779=FACE_OUTER_BOUND('',#1142,.T.);
#780=FACE_OUTER_BOUND('',#1144,.T.);
#781=FACE_OUTER_BOUND('',#1146,.T.);
#782=FACE_OUTER_BOUND('',#1147,.T.);
#783=FACE_OUTER_BOUND('',#1148,.T.);
#784=FACE_OUTER_BOUND('',#1149,.T.);
#785=FACE_OUTER_BOUND('',#1150,.T.);
#786=FACE_OUTER_BOUND('',#1152,.T.);
#787=FACE_OUTER_BOUND('',#1154,.T.);
#788=FACE_OUTER_BOUND('',#1156,.T.);
#789=FACE_OUTER_BOUND('',#1158,.T.);
#790=FACE_OUTER_BOUND('',#1159,.T.);
#791=FACE_OUTER_BOUND('',#1160,.T.);
#792=FACE_OUTER_BOUND('',#1161,.T.);
#793=FACE_OUTER_BOUND('',#1162,.T.);
#794=FACE_OUTER_BOUND('',#1163,.T.);
#795=FACE_OUTER_BOUND('',#1164,.T.);
#796=FACE_OUTER_BOUND('',#1165,.T.);
#797=FACE_OUTER_BOUND('',#1166,.T.);
#798=FACE_OUTER_BOUND('',#1167,.T.);
#799=FACE_OUTER_BOUND('',#1168,.T.);
#800=FACE_OUTER_BOUND('',#1169,.T.);
#801=FACE_OUTER_BOUND('',#1170,.T.);
#802=FACE_OUTER_BOUND('',#1171,.T.);
#803=FACE_OUTER_BOUND('',#1173,.T.);
#804=FACE_OUTER_BOUND('',#1174,.T.);
#805=FACE_OUTER_BOUND('',#1175,.T.);
#806=FACE_OUTER_BOUND('',#1177,.T.);
#807=FACE_OUTER_BOUND('',#1179,.T.);
#808=FACE_OUTER_BOUND('',#1180,.T.);
#809=FACE_OUTER_BOUND('',#1182,.T.);
#810=FACE_OUTER_BOUND('',#1183,.T.);
#811=FACE_OUTER_BOUND('',#1184,.T.);
#812=FACE_OUTER_BOUND('',#1185,.T.);
#813=FACE_OUTER_BOUND('',#1186,.T.);
#814=FACE_OUTER_BOUND('',#1187,.T.);
#815=FACE_OUTER_BOUND('',#1188,.T.);
#816=FACE_OUTER_BOUND('',#1189,.T.);
#817=FACE_OUTER_BOUND('',#1191,.T.);
#818=FACE_OUTER_BOUND('',#1193,.T.);
#819=FACE_OUTER_BOUND('',#1194,.T.);
#820=FACE_OUTER_BOUND('',#1195,.T.);
#821=FACE_OUTER_BOUND('',#1196,.T.);
#822=FACE_OUTER_BOUND('',#1198,.T.);
#823=FACE_OUTER_BOUND('',#1200,.T.);
#824=FACE_OUTER_BOUND('',#1202,.T.);
#825=FACE_OUTER_BOUND('',#1204,.T.);
#826=FACE_OUTER_BOUND('',#1205,.T.);
#827=FACE_OUTER_BOUND('',#1206,.T.);
#828=FACE_OUTER_BOUND('',#1207,.T.);
#829=FACE_OUTER_BOUND('',#1208,.T.);
#830=FACE_OUTER_BOUND('',#1209,.T.);
#831=FACE_OUTER_BOUND('',#1210,.T.);
#832=FACE_OUTER_BOUND('',#1211,.T.);
#833=FACE_OUTER_BOUND('',#1212,.T.);
#834=FACE_OUTER_BOUND('',#1214,.T.);
#835=FACE_OUTER_BOUND('',#1215,.T.);
#836=FACE_OUTER_BOUND('',#1216,.T.);
#837=FACE_OUTER_BOUND('',#1217,.T.);
#838=FACE_OUTER_BOUND('',#1218,.T.);
#839=FACE_OUTER_BOUND('',#1219,.T.);
#840=FACE_OUTER_BOUND('',#1220,.T.);
#841=FACE_OUTER_BOUND('',#1222,.T.);
#842=FACE_OUTER_BOUND('',#1223,.T.);
#843=FACE_OUTER_BOUND('',#1224,.T.);
#844=FACE_OUTER_BOUND('',#1225,.T.);
#845=FACE_OUTER_BOUND('',#1226,.T.);
#846=FACE_OUTER_BOUND('',#1228,.T.);
#847=FACE_OUTER_BOUND('',#1230,.T.);
#848=FACE_OUTER_BOUND('',#1231,.T.);
#849=FACE_OUTER_BOUND('',#1232,.T.);
#850=FACE_OUTER_BOUND('',#1234,.T.);
#851=FACE_OUTER_BOUND('',#1236,.T.);
#852=FACE_OUTER_BOUND('',#1237,.T.);
#853=FACE_OUTER_BOUND('',#1238,.T.);
#854=FACE_OUTER_BOUND('',#1239,.T.);
#855=FACE_OUTER_BOUND('',#1240,.T.);
#856=FACE_OUTER_BOUND('',#1241,.T.);
#857=FACE_OUTER_BOUND('',#1243,.T.);
#858=FACE_OUTER_BOUND('',#1244,.T.);
#859=FACE_OUTER_BOUND('',#1245,.T.);
#860=FACE_OUTER_BOUND('',#1246,.T.);
#861=FACE_OUTER_BOUND('',#1248,.T.);
#862=FACE_OUTER_BOUND('',#1249,.T.);
#863=FACE_OUTER_BOUND('',#1250,.T.);
#864=FACE_OUTER_BOUND('',#1252,.T.);
#865=FACE_OUTER_BOUND('',#1254,.T.);
#866=FACE_OUTER_BOUND('',#1255,.T.);
#867=FACE_OUTER_BOUND('',#1256,.T.);
#868=FACE_OUTER_BOUND('',#1258,.T.);
#869=FACE_OUTER_BOUND('',#1260,.T.);
#870=FACE_OUTER_BOUND('',#1261,.T.);
#871=FACE_OUTER_BOUND('',#1262,.T.);
#872=FACE_OUTER_BOUND('',#1264,.T.);
#873=FACE_OUTER_BOUND('',#1266,.T.);
#874=FACE_OUTER_BOUND('',#1267,.T.);
#875=FACE_OUTER_BOUND('',#1268,.T.);
#876=FACE_OUTER_BOUND('',#1269,.T.);
#877=FACE_OUTER_BOUND('',#1270,.T.);
#878=FACE_OUTER_BOUND('',#1271,.T.);
#879=FACE_OUTER_BOUND('',#1272,.T.);
#880=FACE_OUTER_BOUND('',#1273,.T.);
#881=FACE_OUTER_BOUND('',#1274,.T.);
#882=FACE_OUTER_BOUND('',#1275,.T.);
#883=FACE_OUTER_BOUND('',#1276,.T.);
#884=FACE_OUTER_BOUND('',#1277,.T.);
#885=FACE_OUTER_BOUND('',#1278,.T.);
#886=FACE_OUTER_BOUND('',#1279,.T.);
#887=FACE_OUTER_BOUND('',#1281,.T.);
#888=FACE_OUTER_BOUND('',#1282,.T.);
#889=FACE_OUTER_BOUND('',#1283,.T.);
#890=FACE_OUTER_BOUND('',#1284,.T.);
#891=FACE_OUTER_BOUND('',#1285,.T.);
#892=FACE_OUTER_BOUND('',#1286,.T.);
#893=FACE_OUTER_BOUND('',#1287,.T.);
#894=FACE_OUTER_BOUND('',#1289,.T.);
#895=FACE_OUTER_BOUND('',#1290,.T.);
#896=FACE_OUTER_BOUND('',#1292,.T.);
#897=FACE_OUTER_BOUND('',#1293,.T.);
#898=FACE_OUTER_BOUND('',#1294,.T.);
#899=FACE_OUTER_BOUND('',#1295,.T.);
#900=FACE_OUTER_BOUND('',#1297,.T.);
#901=FACE_OUTER_BOUND('',#1298,.T.);
#902=FACE_OUTER_BOUND('',#1299,.T.);
#903=FACE_OUTER_BOUND('',#1300,.T.);
#904=FACE_OUTER_BOUND('',#1302,.T.);
#905=FACE_OUTER_BOUND('',#1303,.T.);
#906=FACE_OUTER_BOUND('',#1304,.T.);
#907=FACE_OUTER_BOUND('',#1305,.T.);
#908=FACE_OUTER_BOUND('',#1306,.T.);
#909=FACE_OUTER_BOUND('',#1307,.T.);
#910=FACE_OUTER_BOUND('',#1308,.T.);
#911=FACE_OUTER_BOUND('',#1309,.T.);
#912=FACE_OUTER_BOUND('',#1310,.T.);
#913=FACE_OUTER_BOUND('',#1311,.T.);
#914=FACE_OUTER_BOUND('',#1312,.T.);
#915=FACE_OUTER_BOUND('',#1313,.T.);
#916=FACE_OUTER_BOUND('',#1314,.T.);
#917=FACE_OUTER_BOUND('',#1315,.T.);
#918=FACE_OUTER_BOUND('',#1316,.T.);
#919=FACE_OUTER_BOUND('',#1317,.T.);
#920=FACE_OUTER_BOUND('',#1318,.T.);
#921=FACE_OUTER_BOUND('',#1319,.T.);
#922=FACE_OUTER_BOUND('',#1320,.T.);
#923=FACE_OUTER_BOUND('',#1321,.T.);
#924=FACE_OUTER_BOUND('',#1322,.T.);
#925=FACE_OUTER_BOUND('',#1323,.T.);
#926=FACE_OUTER_BOUND('',#1324,.T.);
#927=FACE_OUTER_BOUND('',#1325,.T.);
#928=FACE_OUTER_BOUND('',#1326,.T.);
#929=FACE_OUTER_BOUND('',#1327,.T.);
#930=FACE_OUTER_BOUND('',#1328,.T.);
#931=FACE_OUTER_BOUND('',#1330,.T.);
#932=FACE_OUTER_BOUND('',#1331,.T.);
#933=FACE_OUTER_BOUND('',#1333,.T.);
#934=FACE_OUTER_BOUND('',#1334,.T.);
#935=FACE_OUTER_BOUND('',#1336,.T.);
#936=FACE_OUTER_BOUND('',#1337,.T.);
#937=FACE_OUTER_BOUND('',#1339,.T.);
#938=FACE_OUTER_BOUND('',#1340,.T.);
#939=FACE_OUTER_BOUND('',#1342,.T.);
#940=EDGE_LOOP('',(#3131,#3132,#3133,#3134));
#941=EDGE_LOOP('',(#3135,#3136,#3137,#3138));
#942=EDGE_LOOP('',(#3139,#3140,#3141,#3142));
#943=EDGE_LOOP('',(#3143,#3144,#3145,#3146));
#944=EDGE_LOOP('',(#3147,#3148,#3149,#3150));
#945=EDGE_LOOP('',(#3151,#3152,#3153,#3154));
#946=EDGE_LOOP('',(#3155,#3156,#3157,#3158));
#947=EDGE_LOOP('',(#3159,#3160,#3161,#3162));
#948=EDGE_LOOP('',(#3163,#3164,#3165,#3166));
#949=EDGE_LOOP('',(#3167,#3168,#3169,#3170));
#950=EDGE_LOOP('',(#3171,#3172,#3173,#3174));
#951=EDGE_LOOP('',(#3175));
#952=EDGE_LOOP('',(#3176));
#953=EDGE_LOOP('',(#3177));
#954=EDGE_LOOP('',(#3178));
#955=EDGE_LOOP('',(#3179));
#956=EDGE_LOOP('',(#3180));
#957=EDGE_LOOP('',(#3181,#3182,#3183,#3184));
#958=EDGE_LOOP('',(#3185));
#959=EDGE_LOOP('',(#3186));
#960=EDGE_LOOP('',(#3187));
#961=EDGE_LOOP('',(#3188));
#962=EDGE_LOOP('',(#3189));
#963=EDGE_LOOP('',(#3190));
#964=EDGE_LOOP('',(#3191,#3192,#3193,#3194));
#965=EDGE_LOOP('',(#3195));
#966=EDGE_LOOP('',(#3196));
#967=EDGE_LOOP('',(#3197,#3198,#3199,#3200));
#968=EDGE_LOOP('',(#3201,#3202,#3203,#3204));
#969=EDGE_LOOP('',(#3205,#3206,#3207,#3208,#3209));
#970=EDGE_LOOP('',(#3210,#3211,#3212,#3213,#3214));
#971=EDGE_LOOP('',(#3215,#3216,#3217,#3218,#3219));
#972=EDGE_LOOP('',(#3220,#3221,#3222,#3223,#3224));
#973=EDGE_LOOP('',(#3225,#3226,#3227,#3228,#3229));
#974=EDGE_LOOP('',(#3230,#3231,#3232,#3233,#3234));
#975=EDGE_LOOP('',(#3235,#3236,#3237,#3238,#3239));
#976=EDGE_LOOP('',(#3240,#3241,#3242,#3243,#3244));
#977=EDGE_LOOP('',(#3245,#3246,#3247,#3248));
#978=EDGE_LOOP('',(#3249,#3250));
#979=EDGE_LOOP('',(#3251,#3252));
#980=EDGE_LOOP('',(#3253,#3254));
#981=EDGE_LOOP('',(#3255,#3256));
#982=EDGE_LOOP('',(#3257));
#983=EDGE_LOOP('',(#3258));
#984=EDGE_LOOP('',(#3259));
#985=EDGE_LOOP('',(#3260,#3261,#3262,#3263));
#986=EDGE_LOOP('',(#3264,#3265,#3266,#3267));
#987=EDGE_LOOP('',(#3268,#3269));
#988=EDGE_LOOP('',(#3270,#3271));
#989=EDGE_LOOP('',(#3272,#3273));
#990=EDGE_LOOP('',(#3274,#3275));
#991=EDGE_LOOP('',(#3276));
#992=EDGE_LOOP('',(#3277));
#993=EDGE_LOOP('',(#3278));
#994=EDGE_LOOP('',(#3279,#3280,#3281,#3282));
#995=EDGE_LOOP('',(#3283,#3284,#3285,#3286));
#996=EDGE_LOOP('',(#3287));
#997=EDGE_LOOP('',(#3288));
#998=EDGE_LOOP('',(#3289,#3290,#3291,#3292));
#999=EDGE_LOOP('',(#3293));
#1000=EDGE_LOOP('',(#3294));
#1001=EDGE_LOOP('',(#3295));
#1002=EDGE_LOOP('',(#3296));
#1003=EDGE_LOOP('',(#3297));
#1004=EDGE_LOOP('',(#3298,#3299,#3300,#3301));
#1005=EDGE_LOOP('',(#3302));
#1006=EDGE_LOOP('',(#3303));
#1007=EDGE_LOOP('',(#3304));
#1008=EDGE_LOOP('',(#3305));
#1009=EDGE_LOOP('',(#3306));
#1010=EDGE_LOOP('',(#3307,#3308,#3309,#3310));
#1011=EDGE_LOOP('',(#3311));
#1012=EDGE_LOOP('',(#3312));
#1013=EDGE_LOOP('',(#3313,#3314,#3315,#3316));
#1014=EDGE_LOOP('',(#3317,#3318,#3319,#3320));
#1015=EDGE_LOOP('',(#3321,#3322,#3323,#3324));
#1016=EDGE_LOOP('',(#3325,#3326,#3327,#3328));
#1017=EDGE_LOOP('',(#3329,#3330,#3331,#3332,#3333,#3334,#3335,#3336));
#1018=EDGE_LOOP('',(#3337));
#1019=EDGE_LOOP('',(#3338,#3339,#3340,#3341));
#1020=EDGE_LOOP('',(#3342,#3343,#3344,#3345));
#1021=EDGE_LOOP('',(#3346,#3347,#3348,#3349));
#1022=EDGE_LOOP('',(#3350,#3351,#3352,#3353));
#1023=EDGE_LOOP('',(#3354,#3355,#3356,#3357));
#1024=EDGE_LOOP('',(#3358,#3359,#3360,#3361,#3362,#3363,#3364,#3365));
#1025=EDGE_LOOP('',(#3366));
#1026=EDGE_LOOP('',(#3367,#3368,#3369,#3370));
#1027=EDGE_LOOP('',(#3371,#3372,#3373,#3374));
#1028=EDGE_LOOP('',(#3375,#3376,#3377,#3378));
#1029=EDGE_LOOP('',(#3379,#3380,#3381,#3382));
#1030=EDGE_LOOP('',(#3383,#3384,#3385,#3386,#3387,#3388,#3389,#3390));
#1031=EDGE_LOOP('',(#3391));
#1032=EDGE_LOOP('',(#3392,#3393,#3394,#3395));
#1033=EDGE_LOOP('',(#3396,#3397,#3398,#3399));
#1034=EDGE_LOOP('',(#3400,#3401,#3402,#3403));
#1035=EDGE_LOOP('',(#3404,#3405,#3406,#3407));
#1036=EDGE_LOOP('',(#3408,#3409,#3410,#3411));
#1037=EDGE_LOOP('',(#3412,#3413,#3414,#3415,#3416,#3417,#3418,#3419));
#1038=EDGE_LOOP('',(#3420));
#1039=EDGE_LOOP('',(#3421,#3422,#3423,#3424));
#1040=EDGE_LOOP('',(#3425));
#1041=EDGE_LOOP('',(#3426));
#1042=EDGE_LOOP('',(#3427,#3428,#3429,#3430,#3431,#3432));
#1043=EDGE_LOOP('',(#3433,#3434,#3435,#3436));
#1044=EDGE_LOOP('',(#3437));
#1045=EDGE_LOOP('',(#3438,#3439,#3440,#3441));
#1046=EDGE_LOOP('',(#3442));
#1047=EDGE_LOOP('',(#3443,#3444,#3445,#3446));
#1048=EDGE_LOOP('',(#3447));
#1049=EDGE_LOOP('',(#3448,#3449,#3450,#3451));
#1050=EDGE_LOOP('',(#3452));
#1051=EDGE_LOOP('',(#3453,#3454));
#1052=EDGE_LOOP('',(#3455,#3456,#3457,#3458));
#1053=EDGE_LOOP('',(#3459,#3460,#3461,#3462));
#1054=EDGE_LOOP('',(#3463,#3464));
#1055=EDGE_LOOP('',(#3465,#3466,#3467,#3468));
#1056=EDGE_LOOP('',(#3469,#3470));
#1057=EDGE_LOOP('',(#3471,#3472,#3473,#3474));
#1058=EDGE_LOOP('',(#3475,#3476));
#1059=EDGE_LOOP('',(#3477,#3478,#3479,#3480,#3481,#3482,#3483,#3484,#3485,
#3486,#3487,#3488,#3489,#3490,#3491,#3492,#3493,#3494,#3495,#3496));
#1060=EDGE_LOOP('',(#3497));
#1061=EDGE_LOOP('',(#3498,#3499,#3500,#3501,#3502,#3503,#3504,#3505,#3506));
#1062=EDGE_LOOP('',(#3507));
#1063=EDGE_LOOP('',(#3508));
#1064=EDGE_LOOP('',(#3509));
#1065=EDGE_LOOP('',(#3510));
#1066=EDGE_LOOP('',(#3511,#3512,#3513,#3514));
#1067=EDGE_LOOP('',(#3515,#3516,#3517,#3518));
#1068=EDGE_LOOP('',(#3519,#3520,#3521,#3522));
#1069=EDGE_LOOP('',(#3523,#3524,#3525,#3526));
#1070=EDGE_LOOP('',(#3527,#3528,#3529,#3530));
#1071=EDGE_LOOP('',(#3531));
#1072=EDGE_LOOP('',(#3532));
#1073=EDGE_LOOP('',(#3533,#3534,#3535,#3536));
#1074=EDGE_LOOP('',(#3537,#3538));
#1075=EDGE_LOOP('',(#3539,#3540,#3541,#3542));
#1076=EDGE_LOOP('',(#3543,#3544));
#1077=EDGE_LOOP('',(#3545));
#1078=EDGE_LOOP('',(#3546));
#1079=EDGE_LOOP('',(#3547));
#1080=EDGE_LOOP('',(#3548));
#1081=EDGE_LOOP('',(#3549));
#1082=EDGE_LOOP('',(#3550));
#1083=EDGE_LOOP('',(#3551));
#1084=EDGE_LOOP('',(#3552));
#1085=EDGE_LOOP('',(#3553));
#1086=EDGE_LOOP('',(#3554));
#1087=EDGE_LOOP('',(#3555));
#1088=EDGE_LOOP('',(#3556));
#1089=EDGE_LOOP('',(#3557,#3558,#3559,#3560));
#1090=EDGE_LOOP('',(#3561));
#1091=EDGE_LOOP('',(#3562));
#1092=EDGE_LOOP('',(#3563,#3564,#3565,#3566));
#1093=EDGE_LOOP('',(#3567));
#1094=EDGE_LOOP('',(#3568));
#1095=EDGE_LOOP('',(#3569,#3570,#3571,#3572));
#1096=EDGE_LOOP('',(#3573));
#1097=EDGE_LOOP('',(#3574));
#1098=EDGE_LOOP('',(#3575,#3576,#3577,#3578));
#1099=EDGE_LOOP('',(#3579));
#1100=EDGE_LOOP('',(#3580));
#1101=EDGE_LOOP('',(#3581,#3582,#3583,#3584));
#1102=EDGE_LOOP('',(#3585,#3586,#3587,#3588));
#1103=EDGE_LOOP('',(#3589,#3590,#3591,#3592));
#1104=EDGE_LOOP('',(#3593,#3594,#3595,#3596));
#1105=EDGE_LOOP('',(#3597,#3598,#3599,#3600));
#1106=EDGE_LOOP('',(#3601));
#1107=EDGE_LOOP('',(#3602));
#1108=EDGE_LOOP('',(#3603,#3604,#3605,#3606));
#1109=EDGE_LOOP('',(#3607,#3608,#3609,#3610));
#1110=EDGE_LOOP('',(#3611));
#1111=EDGE_LOOP('',(#3612));
#1112=EDGE_LOOP('',(#3613));
#1113=EDGE_LOOP('',(#3614));
#1114=EDGE_LOOP('',(#3615));
#1115=EDGE_LOOP('',(#3616));
#1116=EDGE_LOOP('',(#3617));
#1117=EDGE_LOOP('',(#3618));
#1118=EDGE_LOOP('',(#3619));
#1119=EDGE_LOOP('',(#3620));
#1120=EDGE_LOOP('',(#3621));
#1121=EDGE_LOOP('',(#3622));
#1122=EDGE_LOOP('',(#3623,#3624,#3625,#3626));
#1123=EDGE_LOOP('',(#3627,#3628,#3629,#3630));
#1124=EDGE_LOOP('',(#3631,#3632,#3633,#3634));
#1125=EDGE_LOOP('',(#3635,#3636,#3637,#3638));
#1126=EDGE_LOOP('',(#3639,#3640,#3641,#3642));
#1127=EDGE_LOOP('',(#3643));
#1128=EDGE_LOOP('',(#3644));
#1129=EDGE_LOOP('',(#3645,#3646,#3647,#3648));
#1130=EDGE_LOOP('',(#3649));
#1131=EDGE_LOOP('',(#3650));
#1132=EDGE_LOOP('',(#3651,#3652,#3653,#3654));
#1133=EDGE_LOOP('',(#3655));
#1134=EDGE_LOOP('',(#3656));
#1135=EDGE_LOOP('',(#3657,#3658,#3659,#3660));
#1136=EDGE_LOOP('',(#3661));
#1137=EDGE_LOOP('',(#3662));
#1138=EDGE_LOOP('',(#3663,#3664,#3665,#3666));
#1139=EDGE_LOOP('',(#3667));
#1140=EDGE_LOOP('',(#3668));
#1141=EDGE_LOOP('',(#3669,#3670,#3671,#3672));
#1142=EDGE_LOOP('',(#3673));
#1143=EDGE_LOOP('',(#3674));
#1144=EDGE_LOOP('',(#3675,#3676,#3677,#3678));
#1145=EDGE_LOOP('',(#3679,#3680,#3681,#3682));
#1146=EDGE_LOOP('',(#3683,#3684,#3685,#3686));
#1147=EDGE_LOOP('',(#3687,#3688,#3689,#3690));
#1148=EDGE_LOOP('',(#3691,#3692,#3693,#3694));
#1149=EDGE_LOOP('',(#3695,#3696,#3697,#3698));
#1150=EDGE_LOOP('',(#3699));
#1151=EDGE_LOOP('',(#3700));
#1152=EDGE_LOOP('',(#3701,#3702,#3703,#3704));
#1153=EDGE_LOOP('',(#3705,#3706,#3707,#3708));
#1154=EDGE_LOOP('',(#3709));
#1155=EDGE_LOOP('',(#3710));
#1156=EDGE_LOOP('',(#3711,#3712,#3713,#3714));
#1157=EDGE_LOOP('',(#3715,#3716,#3717,#3718));
#1158=EDGE_LOOP('',(#3719,#3720,#3721,#3722));
#1159=EDGE_LOOP('',(#3723,#3724,#3725,#3726));
#1160=EDGE_LOOP('',(#3727,#3728,#3729,#3730));
#1161=EDGE_LOOP('',(#3731,#3732,#3733,#3734));
#1162=EDGE_LOOP('',(#3735,#3736,#3737,#3738));
#1163=EDGE_LOOP('',(#3739,#3740,#3741,#3742));
#1164=EDGE_LOOP('',(#3743,#3744,#3745,#3746,#3747,#3748));
#1165=EDGE_LOOP('',(#3749,#3750,#3751,#3752,#3753,#3754));
#1166=EDGE_LOOP('',(#3755));
#1167=EDGE_LOOP('',(#3756));
#1168=EDGE_LOOP('',(#3757,#3758,#3759,#3760));
#1169=EDGE_LOOP('',(#3761,#3762,#3763,#3764));
#1170=EDGE_LOOP('',(#3765,#3766,#3767,#3768));
#1171=EDGE_LOOP('',(#3769));
#1172=EDGE_LOOP('',(#3770));
#1173=EDGE_LOOP('',(#3771,#3772,#3773,#3774));
#1174=EDGE_LOOP('',(#3775,#3776,#3777,#3778));
#1175=EDGE_LOOP('',(#3779));
#1176=EDGE_LOOP('',(#3780));
#1177=EDGE_LOOP('',(#3781));
#1178=EDGE_LOOP('',(#3782));
#1179=EDGE_LOOP('',(#3783,#3784,#3785,#3786));
#1180=EDGE_LOOP('',(#3787));
#1181=EDGE_LOOP('',(#3788));
#1182=EDGE_LOOP('',(#3789,#3790,#3791,#3792));
#1183=EDGE_LOOP('',(#3793,#3794,#3795,#3796));
#1184=EDGE_LOOP('',(#3797,#3798,#3799,#3800));
#1185=EDGE_LOOP('',(#3801));
#1186=EDGE_LOOP('',(#3802));
#1187=EDGE_LOOP('',(#3803,#3804,#3805,#3806));
#1188=EDGE_LOOP('',(#3807,#3808,#3809,#3810));
#1189=EDGE_LOOP('',(#3811));
#1190=EDGE_LOOP('',(#3812));
#1191=EDGE_LOOP('',(#3813));
#1192=EDGE_LOOP('',(#3814));
#1193=EDGE_LOOP('',(#3815,#3816));
#1194=EDGE_LOOP('',(#3817,#3818,#3819,#3820,#3821,#3822,#3823,#3824,#3825));
#1195=EDGE_LOOP('',(#3826,#3827));
#1196=EDGE_LOOP('',(#3828,#3829,#3830,#3831));
#1197=EDGE_LOOP('',(#3832,#3833,#3834,#3835,#3836));
#1198=EDGE_LOOP('',(#3837,#3838,#3839,#3840));
#1199=EDGE_LOOP('',(#3841,#3842));
#1200=EDGE_LOOP('',(#3843));
#1201=EDGE_LOOP('',(#3844));
#1202=EDGE_LOOP('',(#3845));
#1203=EDGE_LOOP('',(#3846));
#1204=EDGE_LOOP('',(#3847));
#1205=EDGE_LOOP('',(#3848,#3849,#3850,#3851));
#1206=EDGE_LOOP('',(#3852,#3853,#3854,#3855));
#1207=EDGE_LOOP('',(#3856,#3857,#3858,#3859));
#1208=EDGE_LOOP('',(#3860,#3861,#3862,#3863));
#1209=EDGE_LOOP('',(#3864,#3865,#3866,#3867));
#1210=EDGE_LOOP('',(#3868,#3869,#3870,#3871));
#1211=EDGE_LOOP('',(#3872,#3873,#3874,#3875,#3876,#3877));
#1212=EDGE_LOOP('',(#3878));
#1213=EDGE_LOOP('',(#3879,#3880,#3881,#3882,#3883,#3884));
#1214=EDGE_LOOP('',(#3885,#3886,#3887,#3888));
#1215=EDGE_LOOP('',(#3889,#3890,#3891,#3892));
#1216=EDGE_LOOP('',(#3893,#3894));
#1217=EDGE_LOOP('',(#3895,#3896));
#1218=EDGE_LOOP('',(#3897,#3898,#3899,#3900));
#1219=EDGE_LOOP('',(#3901,#3902,#3903,#3904));
#1220=EDGE_LOOP('',(#3905,#3906,#3907,#3908,#3909,#3910,#3911,#3912));
#1221=EDGE_LOOP('',(#3913));
#1222=EDGE_LOOP('',(#3914,#3915,#3916,#3917,#3918,#3919,#3920,#3921,#3922,
#3923,#3924,#3925));
#1223=EDGE_LOOP('',(#3926,#3927,#3928,#3929));
#1224=EDGE_LOOP('',(#3930,#3931,#3932,#3933));
#1225=EDGE_LOOP('',(#3934,#3935,#3936,#3937));
#1226=EDGE_LOOP('',(#3938,#3939,#3940,#3941));
#1227=EDGE_LOOP('',(#3942));
#1228=EDGE_LOOP('',(#3943,#3944,#3945,#3946));
#1229=EDGE_LOOP('',(#3947));
#1230=EDGE_LOOP('',(#3948,#3949,#3950,#3951,#3952,#3953,#3954,#3955,#3956,
#3957,#3958,#3959));
#1231=EDGE_LOOP('',(#3960,#3961,#3962,#3963));
#1232=EDGE_LOOP('',(#3964,#3965,#3966,#3967));
#1233=EDGE_LOOP('',(#3968));
#1234=EDGE_LOOP('',(#3969,#3970,#3971,#3972));
#1235=EDGE_LOOP('',(#3973));
#1236=EDGE_LOOP('',(#3974,#3975,#3976,#3977));
#1237=EDGE_LOOP('',(#3978));
#1238=EDGE_LOOP('',(#3979,#3980,#3981,#3982));
#1239=EDGE_LOOP('',(#3983,#3984,#3985,#3986));
#1240=EDGE_LOOP('',(#3987));
#1241=EDGE_LOOP('',(#3988));
#1242=EDGE_LOOP('',(#3989));
#1243=EDGE_LOOP('',(#3990,#3991,#3992,#3993));
#1244=EDGE_LOOP('',(#3994));
#1245=EDGE_LOOP('',(#3995,#3996,#3997,#3998));
#1246=EDGE_LOOP('',(#3999));
#1247=EDGE_LOOP('',(#4000));
#1248=EDGE_LOOP('',(#4001,#4002,#4003,#4004));
#1249=EDGE_LOOP('',(#4005,#4006,#4007,#4008));
#1250=EDGE_LOOP('',(#4009));
#1251=EDGE_LOOP('',(#4010));
#1252=EDGE_LOOP('',(#4011));
#1253=EDGE_LOOP('',(#4012));
#1254=EDGE_LOOP('',(#4013,#4014,#4015,#4016));
#1255=EDGE_LOOP('',(#4017,#4018,#4019,#4020));
#1256=EDGE_LOOP('',(#4021));
#1257=EDGE_LOOP('',(#4022));
#1258=EDGE_LOOP('',(#4023));
#1259=EDGE_LOOP('',(#4024));
#1260=EDGE_LOOP('',(#4025,#4026,#4027,#4028));
#1261=EDGE_LOOP('',(#4029,#4030,#4031,#4032));
#1262=EDGE_LOOP('',(#4033));
#1263=EDGE_LOOP('',(#4034));
#1264=EDGE_LOOP('',(#4035));
#1265=EDGE_LOOP('',(#4036));
#1266=EDGE_LOOP('',(#4037,#4038,#4039,#4040));
#1267=EDGE_LOOP('',(#4041,#4042,#4043,#4044));
#1268=EDGE_LOOP('',(#4045,#4046,#4047,#4048));
#1269=EDGE_LOOP('',(#4049,#4050,#4051,#4052));
#1270=EDGE_LOOP('',(#4053,#4054,#4055,#4056));
#1271=EDGE_LOOP('',(#4057,#4058,#4059,#4060));
#1272=EDGE_LOOP('',(#4061,#4062,#4063,#4064,#4065,#4066));
#1273=EDGE_LOOP('',(#4067,#4068,#4069,#4070,#4071,#4072));
#1274=EDGE_LOOP('',(#4073));
#1275=EDGE_LOOP('',(#4074));
#1276=EDGE_LOOP('',(#4075,#4076,#4077,#4078));
#1277=EDGE_LOOP('',(#4079,#4080,#4081,#4082));
#1278=EDGE_LOOP('',(#4083,#4084,#4085,#4086));
#1279=EDGE_LOOP('',(#4087));
#1280=EDGE_LOOP('',(#4088));
#1281=EDGE_LOOP('',(#4089,#4090,#4091,#4092));
#1282=EDGE_LOOP('',(#4093,#4094,#4095,#4096));
#1283=EDGE_LOOP('',(#4097,#4098,#4099,#4100,#4101,#4102));
#1284=EDGE_LOOP('',(#4103,#4104,#4105,#4106,#4107));
#1285=EDGE_LOOP('',(#4108,#4109,#4110,#4111));
#1286=EDGE_LOOP('',(#4112,#4113,#4114,#4115));
#1287=EDGE_LOOP('',(#4116));
#1288=EDGE_LOOP('',(#4117));
#1289=EDGE_LOOP('',(#4118,#4119,#4120,#4121,#4122));
#1290=EDGE_LOOP('',(#4123));
#1291=EDGE_LOOP('',(#4124));
#1292=EDGE_LOOP('',(#4125,#4126,#4127,#4128));
#1293=EDGE_LOOP('',(#4129,#4130,#4131,#4132,#4133,#4134));
#1294=EDGE_LOOP('',(#4135,#4136,#4137,#4138,#4139));
#1295=EDGE_LOOP('',(#4140));
#1296=EDGE_LOOP('',(#4141));
#1297=EDGE_LOOP('',(#4142,#4143,#4144,#4145));
#1298=EDGE_LOOP('',(#4146,#4147,#4148,#4149));
#1299=EDGE_LOOP('',(#4150,#4151,#4152,#4153));
#1300=EDGE_LOOP('',(#4154));
#1301=EDGE_LOOP('',(#4155));
#1302=EDGE_LOOP('',(#4156,#4157,#4158,#4159,#4160));
#1303=EDGE_LOOP('',(#4161,#4162));
#1304=EDGE_LOOP('',(#4163,#4164));
#1305=EDGE_LOOP('',(#4165,#4166));
#1306=EDGE_LOOP('',(#4167,#4168));
#1307=EDGE_LOOP('',(#4169,#4170));
#1308=EDGE_LOOP('',(#4171,#4172));
#1309=EDGE_LOOP('',(#4173,#4174));
#1310=EDGE_LOOP('',(#4175,#4176));
#1311=EDGE_LOOP('',(#4177,#4178,#4179,#4180));
#1312=EDGE_LOOP('',(#4181,#4182,#4183,#4184,#4185,#4186,#4187,#4188,#4189,
#4190,#4191,#4192,#4193,#4194,#4195,#4196,#4197,#4198,#4199,#4200));
#1313=EDGE_LOOP('',(#4201,#4202,#4203,#4204));
#1314=EDGE_LOOP('',(#4205,#4206,#4207,#4208));
#1315=EDGE_LOOP('',(#4209,#4210,#4211,#4212));
#1316=EDGE_LOOP('',(#4213,#4214,#4215,#4216));
#1317=EDGE_LOOP('',(#4217,#4218,#4219,#4220));
#1318=EDGE_LOOP('',(#4221,#4222,#4223,#4224,#4225,#4226));
#1319=EDGE_LOOP('',(#4227,#4228,#4229,#4230));
#1320=EDGE_LOOP('',(#4231,#4232,#4233,#4234));
#1321=EDGE_LOOP('',(#4235,#4236,#4237,#4238));
#1322=EDGE_LOOP('',(#4239,#4240,#4241,#4242));
#1323=EDGE_LOOP('',(#4243,#4244,#4245,#4246));
#1324=EDGE_LOOP('',(#4247,#4248,#4249,#4250));
#1325=EDGE_LOOP('',(#4251,#4252,#4253,#4254,#4255,#4256,#4257,#4258,#4259,
#4260,#4261,#4262,#4263,#4264,#4265,#4266,#4267,#4268,#4269,#4270));
#1326=EDGE_LOOP('',(#4271,#4272,#4273,#4274));
#1327=EDGE_LOOP('',(#4275,#4276,#4277,#4278));
#1328=EDGE_LOOP('',(#4279));
#1329=EDGE_LOOP('',(#4280));
#1330=EDGE_LOOP('',(#4281,#4282,#4283,#4284));
#1331=EDGE_LOOP('',(#4285));
#1332=EDGE_LOOP('',(#4286));
#1333=EDGE_LOOP('',(#4287,#4288,#4289,#4290));
#1334=EDGE_LOOP('',(#4291));
#1335=EDGE_LOOP('',(#4292));
#1336=EDGE_LOOP('',(#4293,#4294,#4295,#4296));
#1337=EDGE_LOOP('',(#4297));
#1338=EDGE_LOOP('',(#4298));
#1339=EDGE_LOOP('',(#4299,#4300,#4301,#4302));
#1340=EDGE_LOOP('',(#4303));
#1341=EDGE_LOOP('',(#4304));
#1342=EDGE_LOOP('',(#4305,#4306,#4307,#4308));
#1343=LINE('',#7231,#1595);
#1344=LINE('',#7237,#1596);
#1345=LINE('',#7243,#1597);
#1346=LINE('',#7249,#1598);
#1347=LINE('',#7255,#1599);
#1348=LINE('',#7261,#1600);
#1349=LINE('',#7266,#1601);
#1350=LINE('',#7268,#1602);
#1351=LINE('',#7270,#1603);
#1352=LINE('',#7271,#1604);
#1353=LINE('',#7274,#1605);
#1354=LINE('',#7276,#1606);
#1355=LINE('',#7277,#1607);
#1356=LINE('',#7280,#1608);
#1357=LINE('',#7282,#1609);
#1358=LINE('',#7283,#1610);
#1359=LINE('',#7285,#1611);
#1360=LINE('',#7286,#1612);
#1361=LINE('',#7293,#1613);
#1362=LINE('',#7295,#1614);
#1363=LINE('',#7297,#1615);
#1364=LINE('',#7298,#1616);
#1365=LINE('',#7306,#1617);
#1366=LINE('',#7307,#1618);
#1367=LINE('',#7308,#1619);
#1368=LINE('',#7312,#1620);
#1369=LINE('',#7313,#1621);
#1370=LINE('',#7314,#1622);
#1371=LINE('',#7319,#1623);
#1372=LINE('',#7405,#1624);
#1373=LINE('',#7411,#1625);
#1374=LINE('',#7497,#1626);
#1375=LINE('',#7503,#1627);
#1376=LINE('',#7589,#1628);
#1377=LINE('',#7595,#1629);
#1378=LINE('',#7681,#1630);
#1379=LINE('',#7686,#1631);
#1380=LINE('',#7736,#1632);
#1381=LINE('',#7740,#1633);
#1382=LINE('',#7790,#1634);
#1383=LINE('',#7795,#1635);
#1384=LINE('',#7798,#1636);
#1385=LINE('',#7800,#1637);
#1386=LINE('',#7806,#1638);
#1387=LINE('',#7810,#1639);
#1388=LINE('',#7815,#1640);
#1389=LINE('',#7819,#1641);
#1390=LINE('',#7824,#1642);
#1391=LINE('',#7828,#1643);
#1392=LINE('',#7833,#1644);
#1393=LINE('',#7837,#1645);
#1394=LINE('',#7857,#1646);
#1395=LINE('',#7863,#1647);
#1396=LINE('',#7867,#1648);
#1397=LINE('',#7872,#1649);
#1398=LINE('',#7876,#1650);
#1399=LINE('',#7881,#1651);
#1400=LINE('',#7885,#1652);
#1401=LINE('',#7890,#1653);
#1402=LINE('',#7894,#1654);
#1403=LINE('',#7914,#1655);
#1404=LINE('',#9504,#1656);
#1405=LINE('',#9546,#1657);
#1406=LINE('',#9553,#1658);
#1407=LINE('',#9560,#1659);
#1408=LINE('',#9567,#1660);
#1409=LINE('',#9577,#1661);
#1410=LINE('',#9580,#1662);
#1411=LINE('',#9584,#1663);
#1412=LINE('',#9588,#1664);
#1413=LINE('',#9595,#1665);
#1414=LINE('',#9599,#1666);
#1415=LINE('',#9606,#1667);
#1416=LINE('',#9610,#1668);
#1417=LINE('',#9618,#1669);
#1418=LINE('',#9638,#1670);
#1419=LINE('',#9642,#1671);
#1420=LINE('',#9646,#1672);
#1421=LINE('',#9650,#1673);
#1422=LINE('',#9655,#1674);
#1423=LINE('',#9662,#1675);
#1424=LINE('',#9666,#1676);
#1425=LINE('',#9675,#1677);
#1426=LINE('',#9684,#1678);
#1427=LINE('',#9693,#1679);
#1428=LINE('',#9702,#1680);
#1429=LINE('',#9710,#1681);
#1430=LINE('',#9714,#1682);
#1431=LINE('',#9718,#1683);
#1432=LINE('',#9722,#1684);
#1433=LINE('',#9727,#1685);
#1434=LINE('',#9735,#1686);
#1435=LINE('',#9740,#1687);
#1436=LINE('',#9751,#1688);
#1437=LINE('',#9753,#1689);
#1438=LINE('',#9754,#1690);
#1439=LINE('',#9757,#1691);
#1440=LINE('',#9759,#1692);
#1441=LINE('',#9760,#1693);
#1442=LINE('',#9765,#1694);
#1443=LINE('',#9766,#1695);
#1444=LINE('',#9768,#1696);
#1445=LINE('',#9769,#1697);
#1446=LINE('',#9779,#1698);
#1447=LINE('',#9786,#1699);
#1448=LINE('',#9793,#1700);
#1449=LINE('',#9800,#1701);
#1450=LINE('',#9807,#1702);
#1451=LINE('',#9812,#1703);
#1452=LINE('',#9819,#1704);
#1453=LINE('',#9822,#1705);
#1454=LINE('',#9825,#1706);
#1455=LINE('',#9827,#1707);
#1456=LINE('',#9828,#1708);
#1457=LINE('',#9834,#1709);
#1458=LINE('',#9836,#1710);
#1459=LINE('',#9837,#1711);
#1460=LINE('',#9846,#1712);
#1461=LINE('',#9851,#1713);
#1462=LINE('',#9858,#1714);
#1463=LINE('',#9860,#1715);
#1464=LINE('',#9862,#1716);
#1465=LINE('',#9863,#1717);
#1466=LINE('',#9866,#1718);
#1467=LINE('',#9868,#1719);
#1468=LINE('',#9869,#1720);
#1469=LINE('',#9872,#1721);
#1470=LINE('',#9874,#1722);
#1471=LINE('',#9875,#1723);
#1472=LINE('',#9878,#1724);
#1473=LINE('',#9880,#1725);
#1474=LINE('',#9881,#1726);
#1475=LINE('',#9884,#1727);
#1476=LINE('',#9886,#1728);
#1477=LINE('',#9887,#1729);
#1478=LINE('',#9889,#1730);
#1479=LINE('',#9890,#1731);
#1480=LINE('',#9902,#1732);
#1481=LINE('',#9906,#1733);
#1482=LINE('',#9910,#1734);
#1483=LINE('',#9917,#1735);
#1484=LINE('',#9919,#1736);
#1485=LINE('',#9933,#1737);
#1486=LINE('',#9940,#1738);
#1487=LINE('',#9943,#1739);
#1488=LINE('',#9948,#1740);
#1489=LINE('',#9956,#1741);
#1490=LINE('',#9962,#1742);
#1491=LINE('',#9970,#1743);
#1492=LINE('',#10000,#1744);
#1493=LINE('',#10047,#1745);
#1494=LINE('',#10052,#1746);
#1495=LINE('',#10058,#1747);
#1496=LINE('',#10069,#1748);
#1497=LINE('',#10071,#1749);
#1498=LINE('',#10073,#1750);
#1499=LINE('',#10074,#1751);
#1500=LINE('',#10077,#1752);
#1501=LINE('',#10079,#1753);
#1502=LINE('',#10080,#1754);
#1503=LINE('',#10083,#1755);
#1504=LINE('',#10085,#1756);
#1505=LINE('',#10086,#1757);
#1506=LINE('',#10089,#1758);
#1507=LINE('',#10091,#1759);
#1508=LINE('',#10092,#1760);
#1509=LINE('',#10095,#1761);
#1510=LINE('',#10097,#1762);
#1511=LINE('',#10098,#1763);
#1512=LINE('',#10100,#1764);
#1513=LINE('',#10101,#1765);
#1514=LINE('',#10109,#1766);
#1515=LINE('',#10111,#1767);
#1516=LINE('',#10121,#1768);
#1517=LINE('',#10126,#1769);
#1518=LINE('',#10130,#1770);
#1519=LINE('',#10133,#1771);
#1520=LINE('',#10136,#1772);
#1521=LINE('',#10138,#1773);
#1522=LINE('',#10142,#1774);
#1523=LINE('',#10144,#1775);
#1524=LINE('',#10145,#1776);
#1525=LINE('',#10147,#1777);
#1526=LINE('',#10149,#1778);
#1527=LINE('',#10150,#1779);
#1528=LINE('',#10155,#1780);
#1529=LINE('',#10157,#1781);
#1530=LINE('',#10159,#1782);
#1531=LINE('',#10161,#1783);
#1532=LINE('',#10163,#1784);
#1533=LINE('',#10165,#1785);
#1534=LINE('',#10166,#1786);
#1535=LINE('',#10171,#1787);
#1536=LINE('',#10177,#1788);
#1537=LINE('',#10182,#1789);
#1538=LINE('',#10186,#1790);
#1539=LINE('',#10189,#1791);
#1540=LINE('',#10190,#1792);
#1541=LINE('',#10193,#1793);
#1542=LINE('',#10195,#1794);
#1543=LINE('',#10197,#1795);
#1544=LINE('',#10198,#1796);
#1545=LINE('',#10204,#1797);
#1546=LINE('',#10208,#1798);
#1547=LINE('',#10216,#1799);
#1548=LINE('',#10226,#1800);
#1549=LINE('',#10232,#1801);
#1550=LINE('',#10239,#1802);
#1551=LINE('',#10245,#1803);
#1552=LINE('',#10254,#1804);
#1553=LINE('',#10260,#1805);
#1554=LINE('',#10269,#1806);
#1555=LINE('',#10275,#1807);
#1556=LINE('',#10283,#1808);
#1557=LINE('',#10285,#1809);
#1558=LINE('',#10287,#1810);
#1559=LINE('',#10288,#1811);
#1560=LINE('',#10291,#1812);
#1561=LINE('',#10293,#1813);
#1562=LINE('',#10294,#1814);
#1563=LINE('',#10297,#1815);
#1564=LINE('',#10299,#1816);
#1565=LINE('',#10300,#1817);
#1566=LINE('',#10303,#1818);
#1567=LINE('',#10305,#1819);
#1568=LINE('',#10306,#1820);
#1569=LINE('',#10309,#1821);
#1570=LINE('',#10311,#1822);
#1571=LINE('',#10312,#1823);
#1572=LINE('',#10314,#1824);
#1573=LINE('',#10315,#1825);
#1574=LINE('',#10327,#1826);
#1575=LINE('',#10331,#1827);
#1576=LINE('',#10335,#1828);
#1577=LINE('',#10342,#1829);
#1578=LINE('',#10344,#1830);
#1579=LINE('',#10366,#1831);
#1580=LINE('',#10372,#1832);
#1581=LINE('',#10376,#1833);
#1582=LINE('',#10382,#1834);
#1583=LINE('',#10387,#1835);
#1584=LINE('',#10402,#1836);
#1585=LINE('',#10411,#1837);
#1586=LINE('',#10415,#1838);
#1587=LINE('',#10419,#1839);
#1588=LINE('',#10422,#1840);
#1589=LINE('',#10575,#1841);
#1590=LINE('',#10871,#1842);
#1591=LINE('',#10913,#1843);
#1592=LINE('',#10918,#1844);
#1593=LINE('',#10927,#1845);
#1594=LINE('',#10932,#1846);
#1595=VECTOR('',#5678,0.210000000000001);
#1596=VECTOR('',#5685,0.210000000000001);
#1597=VECTOR('',#5692,0.21);
#1598=VECTOR('',#5699,0.21);
#1599=VECTOR('',#5706,0.21);
#1600=VECTOR('',#5713,0.21);
#1601=VECTOR('',#5718,1.);
#1602=VECTOR('',#5719,1.);
#1603=VECTOR('',#5720,1.);
#1604=VECTOR('',#5721,1.);
#1605=VECTOR('',#5724,1.);
#1606=VECTOR('',#5725,1.);
#1607=VECTOR('',#5726,1.);
#1608=VECTOR('',#5729,1.);
#1609=VECTOR('',#5730,1.);
#1610=VECTOR('',#5731,1.);
#1611=VECTOR('',#5734,1.);
#1612=VECTOR('',#5735,1.);
#1613=VECTOR('',#5744,1.);
#1614=VECTOR('',#5745,1.);
#1615=VECTOR('',#5746,1.);
#1616=VECTOR('',#5747,1.);
#1617=VECTOR('',#5754,1.);
#1618=VECTOR('',#5755,1.);
#1619=VECTOR('',#5756,1.);
#1620=VECTOR('',#5759,1.);
#1621=VECTOR('',#5760,1.);
#1622=VECTOR('',#5761,1.);
#1623=VECTOR('',#5766,0.165);
#1624=VECTOR('',#5769,0.165);
#1625=VECTOR('',#5776,0.165);
#1626=VECTOR('',#5779,0.165);
#1627=VECTOR('',#5786,0.165);
#1628=VECTOR('',#5789,0.165);
#1629=VECTOR('',#5796,0.165);
#1630=VECTOR('',#5799,0.165);
#1631=VECTOR('',#5806,0.5);
#1632=VECTOR('',#5815,0.275);
#1633=VECTOR('',#5820,0.5);
#1634=VECTOR('',#5829,0.275);
#1635=VECTOR('',#5834,1.05);
#1636=VECTOR('',#5839,1.);
#1637=VECTOR('',#5842,1.);
#1638=VECTOR('',#5849,1.);
#1639=VECTOR('',#5852,1.);
#1640=VECTOR('',#5857,1.);
#1641=VECTOR('',#5860,1.);
#1642=VECTOR('',#5865,1.);
#1643=VECTOR('',#5868,1.);
#1644=VECTOR('',#5873,1.);
#1645=VECTOR('',#5876,1.);
#1646=VECTOR('',#5911,0.62);
#1647=VECTOR('',#5918,1.);
#1648=VECTOR('',#5921,1.);
#1649=VECTOR('',#5926,1.);
#1650=VECTOR('',#5929,1.);
#1651=VECTOR('',#5934,1.);
#1652=VECTOR('',#5937,1.);
#1653=VECTOR('',#5942,1.);
#1654=VECTOR('',#5945,1.);
#1655=VECTOR('',#5980,0.62);
#1656=VECTOR('',#5997,0.25);
#1657=VECTOR('',#6002,0.165);
#1658=VECTOR('',#6011,0.165);
#1659=VECTOR('',#6020,0.165);
#1660=VECTOR('',#6029,0.165);
#1661=VECTOR('',#6042,1.);
#1662=VECTOR('',#6045,1.);
#1663=VECTOR('',#6048,1.);
#1664=VECTOR('',#6051,1.);
#1665=VECTOR('',#6060,1.);
#1666=VECTOR('',#6063,1.);
#1667=VECTOR('',#6072,1.);
#1668=VECTOR('',#6075,1.);
#1669=VECTOR('',#6086,2.2);
#1670=VECTOR('',#6113,0.275);
#1671=VECTOR('',#6118,0.275);
#1672=VECTOR('',#6123,0.275);
#1673=VECTOR('',#6128,0.275);
#1674=VECTOR('',#6133,1.5);
#1675=VECTOR('',#6142,3.);
#1676=VECTOR('',#6147,1.02);
#1677=VECTOR('',#6160,0.375);
#1678=VECTOR('',#6171,0.375);
#1679=VECTOR('',#6182,0.375);
#1680=VECTOR('',#6193,0.375);
#1681=VECTOR('',#6204,0.225);
#1682=VECTOR('',#6209,0.225);
#1683=VECTOR('',#6214,0.225);
#1684=VECTOR('',#6219,0.225);
#1685=VECTOR('',#6224,1.49);
#1686=VECTOR('',#6235,0.71);
#1687=VECTOR('',#6240,2.2);
#1688=VECTOR('',#6255,1.);
#1689=VECTOR('',#6256,1.);
#1690=VECTOR('',#6257,1.);
#1691=VECTOR('',#6260,1.);
#1692=VECTOR('',#6261,1.);
#1693=VECTOR('',#6262,1.);
#1694=VECTOR('',#6267,1.);
#1695=VECTOR('',#6268,1.);
#1696=VECTOR('',#6271,1.);
#1697=VECTOR('',#6272,1.);
#1698=VECTOR('',#6285,1.05);
#1699=VECTOR('',#6294,1.);
#1700=VECTOR('',#6303,1.05);
#1701=VECTOR('',#6312,1.);
#1702=VECTOR('',#6321,1.05);
#1703=VECTOR('',#6328,0.9);
#1704=VECTOR('',#6335,1.);
#1705=VECTOR('',#6338,1.);
#1706=VECTOR('',#6341,1.);
#1707=VECTOR('',#6342,1.);
#1708=VECTOR('',#6343,1.);
#1709=VECTOR('',#6350,1.);
#1710=VECTOR('',#6353,1.);
#1711=VECTOR('',#6354,1.);
#1712=VECTOR('',#6365,0.895);
#1713=VECTOR('',#6372,0.605);
#1714=VECTOR('',#6381,1.);
#1715=VECTOR('',#6382,1.);
#1716=VECTOR('',#6383,1.);
#1717=VECTOR('',#6384,1.);
#1718=VECTOR('',#6387,1.);
#1719=VECTOR('',#6388,1.);
#1720=VECTOR('',#6389,1.);
#1721=VECTOR('',#6392,1.);
#1722=VECTOR('',#6393,1.);
#1723=VECTOR('',#6394,1.);
#1724=VECTOR('',#6397,1.);
#1725=VECTOR('',#6398,1.);
#1726=VECTOR('',#6399,1.);
#1727=VECTOR('',#6402,1.);
#1728=VECTOR('',#6403,1.);
#1729=VECTOR('',#6404,1.);
#1730=VECTOR('',#6407,1.);
#1731=VECTOR('',#6408,1.);
#1732=VECTOR('',#6425,0.4);
#1733=VECTOR('',#6430,0.425);
#1734=VECTOR('',#6435,0.41);
#1735=VECTOR('',#6444,0.26);
#1736=VECTOR('',#6447,0.25);
#1737=VECTOR('',#6466,2.99742622740447);
#1738=VECTOR('',#6475,0.7);
#1739=VECTOR('',#6478,0.5);
#1740=VECTOR('',#6485,0.5);
#1741=VECTOR('',#6496,0.505);
#1742=VECTOR('',#6503,0.7);
#1743=VECTOR('',#6514,1.);
#1744=VECTOR('',#6521,0.165);
#1745=VECTOR('',#6524,1.);
#1746=VECTOR('',#6529,0.505);
#1747=VECTOR('',#6536,0.9);
#1748=VECTOR('',#6551,1.);
#1749=VECTOR('',#6552,1.);
#1750=VECTOR('',#6553,1.);
#1751=VECTOR('',#6554,1.);
#1752=VECTOR('',#6557,1.);
#1753=VECTOR('',#6558,1.);
#1754=VECTOR('',#6559,1.);
#1755=VECTOR('',#6562,1.);
#1756=VECTOR('',#6563,1.);
#1757=VECTOR('',#6564,1.);
#1758=VECTOR('',#6567,1.);
#1759=VECTOR('',#6568,1.);
#1760=VECTOR('',#6569,1.);
#1761=VECTOR('',#6572,1.);
#1762=VECTOR('',#6573,1.);
#1763=VECTOR('',#6574,1.);
#1764=VECTOR('',#6577,1.);
#1765=VECTOR('',#6578,1.);
#1766=VECTOR('',#6589,0.185);
#1767=VECTOR('',#6592,0.2);
#1768=VECTOR('',#6607,1.);
#1769=VECTOR('',#6612,1.);
#1770=VECTOR('',#6617,1.);
#1771=VECTOR('',#6620,1.);
#1772=VECTOR('',#6623,1.);
#1773=VECTOR('',#6624,1.);
#1774=VECTOR('',#6629,1.);
#1775=VECTOR('',#6630,1.);
#1776=VECTOR('',#6631,1.);
#1777=VECTOR('',#6632,1.);
#1778=VECTOR('',#6633,1.);
#1779=VECTOR('',#6634,1.);
#1780=VECTOR('',#6639,1.);
#1781=VECTOR('',#6640,1.);
#1782=VECTOR('',#6641,1.);
#1783=VECTOR('',#6642,1.);
#1784=VECTOR('',#6643,1.);
#1785=VECTOR('',#6644,1.);
#1786=VECTOR('',#6645,1.);
#1787=VECTOR('',#6650,0.51);
#1788=VECTOR('',#6657,0.51);
#1789=VECTOR('',#6662,1.);
#1790=VECTOR('',#6669,1.);
#1791=VECTOR('',#6672,1.);
#1792=VECTOR('',#6673,1.);
#1793=VECTOR('',#6676,1.);
#1794=VECTOR('',#6677,1.);
#1795=VECTOR('',#6678,1.);
#1796=VECTOR('',#6679,1.);
#1797=VECTOR('',#6690,1.);
#1798=VECTOR('',#6695,0.6);
#1799=VECTOR('',#6706,0.165);
#1800=VECTOR('',#6719,0.7);
#1801=VECTOR('',#6728,0.5);
#1802=VECTOR('',#6737,0.505);
#1803=VECTOR('',#6744,0.7);
#1804=VECTOR('',#6757,0.505);
#1805=VECTOR('',#6764,0.7);
#1806=VECTOR('',#6777,0.225);
#1807=VECTOR('',#6784,0.7);
#1808=VECTOR('',#6795,1.);
#1809=VECTOR('',#6796,1.);
#1810=VECTOR('',#6797,1.);
#1811=VECTOR('',#6798,1.);
#1812=VECTOR('',#6801,1.);
#1813=VECTOR('',#6802,1.);
#1814=VECTOR('',#6803,1.);
#1815=VECTOR('',#6806,1.);
#1816=VECTOR('',#6807,1.);
#1817=VECTOR('',#6808,1.);
#1818=VECTOR('',#6811,1.);
#1819=VECTOR('',#6812,1.);
#1820=VECTOR('',#6813,1.);
#1821=VECTOR('',#6816,1.);
#1822=VECTOR('',#6817,1.);
#1823=VECTOR('',#6818,1.);
#1824=VECTOR('',#6821,1.);
#1825=VECTOR('',#6822,1.);
#1826=VECTOR('',#6839,0.325);
#1827=VECTOR('',#6844,0.35);
#1828=VECTOR('',#6849,0.335);
#1829=VECTOR('',#6858,0.21);
#1830=VECTOR('',#6861,0.2);
#1831=VECTOR('',#6894,0.976185);
#1832=VECTOR('',#6901,0.5);
#1833=VECTOR('',#6906,0.53);
#1834=VECTOR('',#6915,0.976185);
#1835=VECTOR('',#6922,0.53);
#1836=VECTOR('',#6941,1.023815);
#1837=VECTOR('',#6952,1.47);
#1838=VECTOR('',#6957,1.5);
#1839=VECTOR('',#6962,1.47);
#1840=VECTOR('',#6967,1.023815);
#1841=VECTOR('',#7018,1.019052);
#1842=VECTOR('',#7095,0.980948);
#1843=VECTOR('',#7124,1.013815);
#1844=VECTOR('',#7131,0.991185);
#1845=VECTOR('',#7142,1.013815);
#1846=VECTOR('',#7149,0.991185);
#1847=CIRCLE('',#5020,0.210000000000001);
#1848=CIRCLE('',#5021,0.210000000000001);
#1849=CIRCLE('',#5023,0.210000000000001);
#1850=CIRCLE('',#5024,0.210000000000001);
#1851=CIRCLE('',#5026,0.21);
#1852=CIRCLE('',#5027,0.21);
#1853=CIRCLE('',#5029,0.21);
#1854=CIRCLE('',#5030,0.21);
#1855=CIRCLE('',#5032,0.21);
#1856=CIRCLE('',#5033,0.21);
#1857=CIRCLE('',#5035,0.21);
#1858=CIRCLE('',#5036,0.21);
#1859=CIRCLE('',#5045,0.5);
#1860=CIRCLE('',#5046,0.5);
#1861=CIRCLE('',#5050,0.165);
#1862=CIRCLE('',#5052,0.165);
#1863=CIRCLE('',#5054,0.165);
#1864=CIRCLE('',#5056,0.165);
#1865=CIRCLE('',#5058,0.165);
#1866=CIRCLE('',#5060,0.165);
#1867=CIRCLE('',#5062,0.165);
#1868=CIRCLE('',#5064,0.165);
#1869=CIRCLE('',#5066,0.5);
#1870=CIRCLE('',#5068,0.275);
#1871=CIRCLE('',#5070,0.275);
#1872=CIRCLE('',#5072,0.5);
#1873=CIRCLE('',#5074,0.275);
#1874=CIRCLE('',#5076,0.275);
#1875=CIRCLE('',#5078,1.05);
#1876=CIRCLE('',#5079,1.05);
#1877=CIRCLE('',#5085,0.225);
#1878=CIRCLE('',#5086,0.225);
#1879=CIRCLE('',#5088,0.225);
#1880=CIRCLE('',#5089,0.225);
#1881=CIRCLE('',#5091,0.225);
#1882=CIRCLE('',#5092,0.225);
#1883=CIRCLE('',#5094,0.225);
#1884=CIRCLE('',#5095,0.225);
#1885=CIRCLE('',#5097,1.9);
#1886=CIRCLE('',#5098,1.9);
#1887=CIRCLE('',#5099,1.9);
#1888=CIRCLE('',#5100,1.9);
#1889=CIRCLE('',#5101,0.62);
#1890=CIRCLE('',#5103,1.9);
#1891=CIRCLE('',#5105,1.9);
#1892=CIRCLE('',#5107,1.9);
#1893=CIRCLE('',#5109,1.9);
#1894=CIRCLE('',#5111,0.62);
#1895=CIRCLE('',#5115,0.225);
#1896=CIRCLE('',#5116,0.225);
#1897=CIRCLE('',#5118,0.225);
#1898=CIRCLE('',#5119,0.225);
#1899=CIRCLE('',#5121,0.225);
#1900=CIRCLE('',#5122,0.225);
#1901=CIRCLE('',#5124,0.225);
#1902=CIRCLE('',#5125,0.225);
#1903=CIRCLE('',#5127,1.9);
#1904=CIRCLE('',#5128,1.9);
#1905=CIRCLE('',#5129,1.9);
#1906=CIRCLE('',#5130,1.9);
#1907=CIRCLE('',#5131,0.62);
#1908=CIRCLE('',#5133,1.9);
#1909=CIRCLE('',#5135,1.9);
#1910=CIRCLE('',#5137,1.9);
#1911=CIRCLE('',#5139,1.9);
#1912=CIRCLE('',#5141,0.62);
#1913=CIRCLE('',#5144,0.08);
#1914=CIRCLE('',#5145,0.08);
#1915=CIRCLE('',#5151,0.165);
#1916=CIRCLE('',#5152,0.165);
#1917=CIRCLE('',#5155,0.165);
#1918=CIRCLE('',#5156,0.165);
#1919=CIRCLE('',#5159,0.165);
#1920=CIRCLE('',#5160,0.165);
#1921=CIRCLE('',#5163,0.165);
#1922=CIRCLE('',#5164,0.165);
#1923=CIRCLE('',#5167,2.2);
#1924=CIRCLE('',#5168,0.525);
#1925=CIRCLE('',#5170,0.525);
#1926=CIRCLE('',#5172,0.525);
#1927=CIRCLE('',#5173,0.525);
#1928=CIRCLE('',#5175,2.2);
#1929=CIRCLE('',#5177,0.525);
#1930=CIRCLE('',#5178,0.525);
#1931=CIRCLE('',#5180,2.2);
#1932=CIRCLE('',#5182,0.525);
#1933=CIRCLE('',#5183,0.525);
#1934=CIRCLE('',#5185,2.2);
#1935=CIRCLE('',#5187,2.2);
#1936=CIRCLE('',#5188,2.2);
#1937=CIRCLE('',#5189,2.2);
#1938=CIRCLE('',#5190,2.2);
#1939=CIRCLE('',#5191,2.2);
#1940=CIRCLE('',#5192,2.2);
#1941=CIRCLE('',#5194,3.);
#1942=CIRCLE('',#5195,0.275);
#1943=CIRCLE('',#5196,0.275);
#1944=CIRCLE('',#5197,0.275);
#1945=CIRCLE('',#5198,0.275);
#1946=CIRCLE('',#5200,0.275);
#1947=CIRCLE('',#5202,0.275);
#1948=CIRCLE('',#5204,0.275);
#1949=CIRCLE('',#5206,0.275);
#1950=CIRCLE('',#5208,1.5);
#1951=CIRCLE('',#5209,1.5);
#1952=CIRCLE('',#5211,1.02);
#1953=CIRCLE('',#5213,3.);
#1954=CIRCLE('',#5215,1.02);
#1955=CIRCLE('',#5220,0.375);
#1956=CIRCLE('',#5221,0.375);
#1957=CIRCLE('',#5223,0.225);
#1958=CIRCLE('',#5225,0.375);
#1959=CIRCLE('',#5226,0.375);
#1960=CIRCLE('',#5228,0.225);
#1961=CIRCLE('',#5230,0.375);
#1962=CIRCLE('',#5231,0.375);
#1963=CIRCLE('',#5233,0.225);
#1964=CIRCLE('',#5235,0.375);
#1965=CIRCLE('',#5236,0.375);
#1966=CIRCLE('',#5238,0.225);
#1967=CIRCLE('',#5240,0.225);
#1968=CIRCLE('',#5242,0.225);
#1969=CIRCLE('',#5244,0.225);
#1970=CIRCLE('',#5246,0.225);
#1971=CIRCLE('',#5248,1.49);
#1972=CIRCLE('',#5249,1.49);
#1973=CIRCLE('',#5251,0.71);
#1974=CIRCLE('',#5253,0.71);
#1975=CIRCLE('',#5255,2.2);
#1976=CIRCLE('',#5256,2.2);
#1977=CIRCLE('',#5262,0.9);
#1978=CIRCLE('',#5265,0.9);
#1979=CIRCLE('',#5269,1.05);
#1980=CIRCLE('',#5270,0.9);
#1981=CIRCLE('',#5272,1.05);
#1982=CIRCLE('',#5274,1.);
#1983=CIRCLE('',#5276,1.);
#1984=CIRCLE('',#5278,1.05);
#1985=CIRCLE('',#5280,1.05);
#1986=CIRCLE('',#5282,1.);
#1987=CIRCLE('',#5284,1.);
#1988=CIRCLE('',#5286,1.05);
#1989=CIRCLE('',#5288,1.05);
#1990=CIRCLE('',#5290,0.9);
#1991=CIRCLE('',#5294,0.895);
#1992=CIRCLE('',#5295,0.605);
#1993=CIRCLE('',#5298,0.895);
#1994=CIRCLE('',#5299,0.605);
#1995=CIRCLE('',#5302,0.895);
#1996=CIRCLE('',#5303,0.605);
#1997=CIRCLE('',#5305,0.895);
#1998=CIRCLE('',#5307,0.605);
#1999=CIRCLE('',#5321,0.24505);
#2000=CIRCLE('',#5323,0.375);
#2001=CIRCLE('',#5325,0.425);
#2002=CIRCLE('',#5327,0.425);
#2003=CIRCLE('',#5329,0.395);
#2004=CIRCLE('',#5331,0.27);
#2005=CIRCLE('',#5333,0.24505);
#2006=CIRCLE('',#5338,2.99742622740447);
#2007=CIRCLE('',#5339,0.5);
#2008=CIRCLE('',#5341,2.99742622740447);
#2009=CIRCLE('',#5342,0.7);
#2010=CIRCLE('',#5345,0.7);
#2011=CIRCLE('',#5346,0.5);
#2012=CIRCLE('',#5349,0.5);
#2013=CIRCLE('',#5351,0.5);
#2014=CIRCLE('',#5356,0.505);
#2015=CIRCLE('',#5357,0.505);
#2016=CIRCLE('',#5359,0.7);
#2017=CIRCLE('',#5360,0.7);
#2018=CIRCLE('',#5365,0.165);
#2019=CIRCLE('',#5367,0.165);
#2020=CIRCLE('',#5370,0.505);
#2021=CIRCLE('',#5371,0.505);
#2022=CIRCLE('',#5373,0.9);
#2023=CIRCLE('',#5374,0.9);
#2024=CIRCLE('',#5379,0.1954);
#2025=CIRCLE('',#5388,0.17);
#2026=CIRCLE('',#5390,0.1954);
#2027=CIRCLE('',#5399,1.);
#2028=CIRCLE('',#5401,1.);
#2029=CIRCLE('',#5403,1.);
#2030=CIRCLE('',#5405,1.);
#2031=CIRCLE('',#5407,0.6);
#2032=CIRCLE('',#5410,0.51);
#2033=CIRCLE('',#5411,0.51);
#2034=CIRCLE('',#5413,0.51);
#2035=CIRCLE('',#5414,0.51);
#2036=CIRCLE('',#5416,0.6);
#2037=CIRCLE('',#5417,0.6);
#2038=CIRCLE('',#5422,0.6);
#2039=CIRCLE('',#5423,0.6);
#2040=CIRCLE('',#5427,0.6);
#2041=CIRCLE('',#5432,0.165);
#2042=CIRCLE('',#5433,0.165);
#2043=CIRCLE('',#5436,0.7);
#2044=CIRCLE('',#5437,0.5);
#2045=CIRCLE('',#5439,0.7);
#2046=CIRCLE('',#5442,0.5);
#2047=CIRCLE('',#5446,0.505);
#2048=CIRCLE('',#5447,0.505);
#2049=CIRCLE('',#5449,0.7);
#2050=CIRCLE('',#5450,0.7);
#2051=CIRCLE('',#5455,0.505);
#2052=CIRCLE('',#5456,0.505);
#2053=CIRCLE('',#5458,0.7);
#2054=CIRCLE('',#5459,0.7);
#2055=CIRCLE('',#5464,0.225);
#2056=CIRCLE('',#5465,0.225);
#2057=CIRCLE('',#5467,0.7);
#2058=CIRCLE('',#5468,0.7);
#2059=CIRCLE('',#5481,0.1954);
#2060=CIRCLE('',#5483,0.3);
#2061=CIRCLE('',#5485,0.35);
#2062=CIRCLE('',#5487,0.35);
#2063=CIRCLE('',#5489,0.32);
#2064=CIRCLE('',#5491,0.22);
#2065=CIRCLE('',#5493,0.1954);
#2066=CIRCLE('',#5505,0.976185);
#2067=CIRCLE('',#5506,0.976185);
#2068=CIRCLE('',#5507,0.247676);
#2069=CIRCLE('',#5508,0.976185);
#2070=CIRCLE('',#5509,0.976185);
#2071=CIRCLE('',#5511,0.976185);
#2072=CIRCLE('',#5513,0.5);
#2073=CIRCLE('',#5514,0.5);
#2074=CIRCLE('',#5516,0.56);
#2075=CIRCLE('',#5519,0.976185);
#2076=CIRCLE('',#5521,0.56);
#2077=CIRCLE('',#5525,1.023815);
#2078=CIRCLE('',#5526,1.023815);
#2079=CIRCLE('',#5527,0.247676);
#2080=CIRCLE('',#5528,1.023815);
#2081=CIRCLE('',#5529,1.023815);
#2082=CIRCLE('',#5531,1.023815);
#2083=CIRCLE('',#5533,1.44);
#2084=CIRCLE('',#5534,1.023815);
#2085=CIRCLE('',#5536,1.5);
#2086=CIRCLE('',#5538,1.5);
#2087=CIRCLE('',#5540,1.44);
#2088=CIRCLE('',#5545,0.23815);
#2089=CIRCLE('',#5547,0.23815);
#2090=CIRCLE('',#5549,0.23815);
#2091=CIRCLE('',#5551,0.23815);
#2092=CIRCLE('',#5553,0.23815);
#2093=CIRCLE('',#5555,0.23815);
#2094=CIRCLE('',#5557,0.23815);
#2095=CIRCLE('',#5559,0.23815);
#2096=CIRCLE('',#5562,0.243053047864041);
#2097=CIRCLE('',#5563,0.243053047864041);
#2098=CIRCLE('',#5565,1.019052);
#2099=CIRCLE('',#5566,1.019052);
#2100=CIRCLE('',#5567,1.019052);
#2101=CIRCLE('',#5568,1.019052);
#2102=CIRCLE('',#5569,1.019052);
#2103=CIRCLE('',#5570,1.019052);
#2104=CIRCLE('',#5571,1.019052);
#2105=CIRCLE('',#5572,1.019052);
#2106=CIRCLE('',#5573,1.019052);
#2107=CIRCLE('',#5575,0.980948);
#2108=CIRCLE('',#5576,0.243053047864041);
#2109=CIRCLE('',#5578,0.243053047864041);
#2110=CIRCLE('',#5580,0.980948);
#2111=CIRCLE('',#5581,0.243053047864041);
#2112=CIRCLE('',#5583,0.243053047864041);
#2113=CIRCLE('',#5585,0.980948);
#2114=CIRCLE('',#5586,0.243053047864041);
#2115=CIRCLE('',#5588,0.243053047864041);
#2116=CIRCLE('',#5590,0.980948);
#2117=CIRCLE('',#5591,0.243053047864041);
#2118=CIRCLE('',#5593,0.243053047864041);
#2119=CIRCLE('',#5595,0.980948);
#2120=CIRCLE('',#5596,0.243053047864041);
#2121=CIRCLE('',#5598,0.243053047864041);
#2122=CIRCLE('',#5600,0.980948);
#2123=CIRCLE('',#5601,0.243053047864041);
#2124=CIRCLE('',#5603,0.243053047864041);
#2125=CIRCLE('',#5605,0.980948);
#2126=CIRCLE('',#5606,0.980948);
#2127=CIRCLE('',#5607,0.980948);
#2128=CIRCLE('',#5609,0.243053047864041);
#2129=CIRCLE('',#5611,0.243053047864041);
#2130=CIRCLE('',#5616,1.013815);
#2131=CIRCLE('',#5617,0.991185);
#2132=CIRCLE('',#5619,1.013815);
#2133=CIRCLE('',#5621,0.991185);
#2134=CIRCLE('',#5624,1.013815);
#2135=CIRCLE('',#5625,0.991185);
#2136=CIRCLE('',#5627,1.013815);
#2137=CIRCLE('',#5629,0.991185);
#2138=VERTEX_POINT('',#7228);
#2139=VERTEX_POINT('',#7230);
#2140=VERTEX_POINT('',#7234);
#2141=VERTEX_POINT('',#7236);
#2142=VERTEX_POINT('',#7240);
#2143=VERTEX_POINT('',#7242);
#2144=VERTEX_POINT('',#7246);
#2145=VERTEX_POINT('',#7248);
#2146=VERTEX_POINT('',#7252);
#2147=VERTEX_POINT('',#7254);
#2148=VERTEX_POINT('',#7258);
#2149=VERTEX_POINT('',#7260);
#2150=VERTEX_POINT('',#7264);
#2151=VERTEX_POINT('',#7265);
#2152=VERTEX_POINT('',#7267);
#2153=VERTEX_POINT('',#7269);
#2154=VERTEX_POINT('',#7273);
#2155=VERTEX_POINT('',#7275);
#2156=VERTEX_POINT('',#7279);
#2157=VERTEX_POINT('',#7281);
#2158=VERTEX_POINT('',#7291);
#2159=VERTEX_POINT('',#7292);
#2160=VERTEX_POINT('',#7294);
#2161=VERTEX_POINT('',#7296);
#2162=VERTEX_POINT('',#7299);
#2163=VERTEX_POINT('',#7301);
#2164=VERTEX_POINT('',#7304);
#2165=VERTEX_POINT('',#7305);
#2166=VERTEX_POINT('',#7310);
#2167=VERTEX_POINT('',#7311);
#2168=VERTEX_POINT('',#7316);
#2169=VERTEX_POINT('',#7318);
#2170=VERTEX_POINT('',#7320);
#2171=VERTEX_POINT('',#7362);
#2172=VERTEX_POINT('',#7363);
#2173=VERTEX_POINT('',#7404);
#2174=VERTEX_POINT('',#7408);
#2175=VERTEX_POINT('',#7410);
#2176=VERTEX_POINT('',#7412);
#2177=VERTEX_POINT('',#7454);
#2178=VERTEX_POINT('',#7455);
#2179=VERTEX_POINT('',#7496);
#2180=VERTEX_POINT('',#7500);
#2181=VERTEX_POINT('',#7502);
#2182=VERTEX_POINT('',#7504);
#2183=VERTEX_POINT('',#7546);
#2184=VERTEX_POINT('',#7547);
#2185=VERTEX_POINT('',#7588);
#2186=VERTEX_POINT('',#7592);
#2187=VERTEX_POINT('',#7594);
#2188=VERTEX_POINT('',#7596);
#2189=VERTEX_POINT('',#7638);
#2190=VERTEX_POINT('',#7639);
#2191=VERTEX_POINT('',#7680);
#2192=VERTEX_POINT('',#7684);
#2193=VERTEX_POINT('',#7687);
#2194=VERTEX_POINT('',#7731);
#2195=VERTEX_POINT('',#7734);
#2196=VERTEX_POINT('',#7738);
#2197=VERTEX_POINT('',#7741);
#2198=VERTEX_POINT('',#7785);
#2199=VERTEX_POINT('',#7788);
#2200=VERTEX_POINT('',#7792);
#2201=VERTEX_POINT('',#7794);
#2202=VERTEX_POINT('',#7804);
#2203=VERTEX_POINT('',#7805);
#2204=VERTEX_POINT('',#7807);
#2205=VERTEX_POINT('',#7809);
#2206=VERTEX_POINT('',#7813);
#2207=VERTEX_POINT('',#7814);
#2208=VERTEX_POINT('',#7816);
#2209=VERTEX_POINT('',#7818);
#2210=VERTEX_POINT('',#7822);
#2211=VERTEX_POINT('',#7823);
#2212=VERTEX_POINT('',#7825);
#2213=VERTEX_POINT('',#7827);
#2214=VERTEX_POINT('',#7831);
#2215=VERTEX_POINT('',#7832);
#2216=VERTEX_POINT('',#7834);
#2217=VERTEX_POINT('',#7836);
#2218=VERTEX_POINT('',#7844);
#2219=VERTEX_POINT('',#7855);
#2220=VERTEX_POINT('',#7861);
#2221=VERTEX_POINT('',#7862);
#2222=VERTEX_POINT('',#7864);
#2223=VERTEX_POINT('',#7866);
#2224=VERTEX_POINT('',#7870);
#2225=VERTEX_POINT('',#7871);
#2226=VERTEX_POINT('',#7873);
#2227=VERTEX_POINT('',#7875);
#2228=VERTEX_POINT('',#7879);
#2229=VERTEX_POINT('',#7880);
#2230=VERTEX_POINT('',#7882);
#2231=VERTEX_POINT('',#7884);
#2232=VERTEX_POINT('',#7888);
#2233=VERTEX_POINT('',#7889);
#2234=VERTEX_POINT('',#7891);
#2235=VERTEX_POINT('',#7893);
#2236=VERTEX_POINT('',#7901);
#2237=VERTEX_POINT('',#7912);
#2238=VERTEX_POINT('',#9317);
#2239=VERTEX_POINT('',#9319);
#2240=VERTEX_POINT('',#9465);
#2241=VERTEX_POINT('',#9466);
#2242=VERTEX_POINT('',#9503);
#2243=VERTEX_POINT('',#9505);
#2244=VERTEX_POINT('',#9543);
#2245=VERTEX_POINT('',#9545);
#2246=VERTEX_POINT('',#9550);
#2247=VERTEX_POINT('',#9552);
#2248=VERTEX_POINT('',#9557);
#2249=VERTEX_POINT('',#9559);
#2250=VERTEX_POINT('',#9564);
#2251=VERTEX_POINT('',#9566);
#2252=VERTEX_POINT('',#9571);
#2253=VERTEX_POINT('',#9572);
#2254=VERTEX_POINT('',#9576);
#2255=VERTEX_POINT('',#9578);
#2256=VERTEX_POINT('',#9582);
#2257=VERTEX_POINT('',#9583);
#2258=VERTEX_POINT('',#9585);
#2259=VERTEX_POINT('',#9587);
#2260=VERTEX_POINT('',#9593);
#2261=VERTEX_POINT('',#9594);
#2262=VERTEX_POINT('',#9596);
#2263=VERTEX_POINT('',#9598);
#2264=VERTEX_POINT('',#9604);
#2265=VERTEX_POINT('',#9605);
#2266=VERTEX_POINT('',#9607);
#2267=VERTEX_POINT('',#9609);
#2268=VERTEX_POINT('',#9615);
#2269=VERTEX_POINT('',#9617);
#2270=VERTEX_POINT('',#9625);
#2271=VERTEX_POINT('',#9627);
#2272=VERTEX_POINT('',#9629);
#2273=VERTEX_POINT('',#9631);
#2274=VERTEX_POINT('',#9633);
#2275=VERTEX_POINT('',#9636);
#2276=VERTEX_POINT('',#9640);
#2277=VERTEX_POINT('',#9644);
#2278=VERTEX_POINT('',#9648);
#2279=VERTEX_POINT('',#9652);
#2280=VERTEX_POINT('',#9654);
#2281=VERTEX_POINT('',#9658);
#2282=VERTEX_POINT('',#9661);
#2283=VERTEX_POINT('',#9665);
#2284=VERTEX_POINT('',#9672);
#2285=VERTEX_POINT('',#9674);
#2286=VERTEX_POINT('',#9678);
#2287=VERTEX_POINT('',#9681);
#2288=VERTEX_POINT('',#9683);
#2289=VERTEX_POINT('',#9687);
#2290=VERTEX_POINT('',#9690);
#2291=VERTEX_POINT('',#9692);
#2292=VERTEX_POINT('',#9696);
#2293=VERTEX_POINT('',#9699);
#2294=VERTEX_POINT('',#9701);
#2295=VERTEX_POINT('',#9705);
#2296=VERTEX_POINT('',#9708);
#2297=VERTEX_POINT('',#9712);
#2298=VERTEX_POINT('',#9716);
#2299=VERTEX_POINT('',#9720);
#2300=VERTEX_POINT('',#9724);
#2301=VERTEX_POINT('',#9726);
#2302=VERTEX_POINT('',#9730);
#2303=VERTEX_POINT('',#9733);
#2304=VERTEX_POINT('',#9737);
#2305=VERTEX_POINT('',#9739);
#2306=VERTEX_POINT('',#9747);
#2307=VERTEX_POINT('',#9748);
#2308=VERTEX_POINT('',#9750);
#2309=VERTEX_POINT('',#9752);
#2310=VERTEX_POINT('',#9756);
#2311=VERTEX_POINT('',#9758);
#2312=VERTEX_POINT('',#9762);
#2313=VERTEX_POINT('',#9764);
#2314=VERTEX_POINT('',#9772);
#2315=VERTEX_POINT('',#9774);
#2316=VERTEX_POINT('',#9777);
#2317=VERTEX_POINT('',#9781);
#2318=VERTEX_POINT('',#9784);
#2319=VERTEX_POINT('',#9788);
#2320=VERTEX_POINT('',#9791);
#2321=VERTEX_POINT('',#9795);
#2322=VERTEX_POINT('',#9798);
#2323=VERTEX_POINT('',#9802);
#2324=VERTEX_POINT('',#9805);
#2325=VERTEX_POINT('',#9809);
#2326=VERTEX_POINT('',#9815);
#2327=VERTEX_POINT('',#9816);
#2328=VERTEX_POINT('',#9818);
#2329=VERTEX_POINT('',#9820);
#2330=VERTEX_POINT('',#9824);
#2331=VERTEX_POINT('',#9826);
#2332=VERTEX_POINT('',#9830);
#2333=VERTEX_POINT('',#9832);
#2334=VERTEX_POINT('',#9839);
#2335=VERTEX_POINT('',#9841);
#2336=VERTEX_POINT('',#9844);
#2337=VERTEX_POINT('',#9848);
#2338=VERTEX_POINT('',#9856);
#2339=VERTEX_POINT('',#9857);
#2340=VERTEX_POINT('',#9859);
#2341=VERTEX_POINT('',#9861);
#2342=VERTEX_POINT('',#9865);
#2343=VERTEX_POINT('',#9867);
#2344=VERTEX_POINT('',#9871);
#2345=VERTEX_POINT('',#9873);
#2346=VERTEX_POINT('',#9877);
#2347=VERTEX_POINT('',#9879);
#2348=VERTEX_POINT('',#9883);
#2349=VERTEX_POINT('',#9885);
#2350=VERTEX_POINT('',#9894);
#2351=VERTEX_POINT('',#9897);
#2352=VERTEX_POINT('',#9900);
#2353=VERTEX_POINT('',#9904);
#2354=VERTEX_POINT('',#9908);
#2355=VERTEX_POINT('',#9912);
#2356=VERTEX_POINT('',#9915);
#2357=VERTEX_POINT('',#9923);
#2358=VERTEX_POINT('',#9925);
#2359=VERTEX_POINT('',#9928);
#2360=VERTEX_POINT('',#9930);
#2361=VERTEX_POINT('',#9935);
#2362=VERTEX_POINT('',#9937);
#2363=VERTEX_POINT('',#9942);
#2364=VERTEX_POINT('',#9946);
#2365=VERTEX_POINT('',#9953);
#2366=VERTEX_POINT('',#9955);
#2367=VERTEX_POINT('',#9959);
#2368=VERTEX_POINT('',#9961);
#2369=VERTEX_POINT('',#9968);
#2370=VERTEX_POINT('',#9969);
#2371=VERTEX_POINT('',#9973);
#2372=VERTEX_POINT('',#9988);
#2373=VERTEX_POINT('',#9990);
#2374=VERTEX_POINT('',#9999);
#2375=VERTEX_POINT('',#10001);
#2376=VERTEX_POINT('',#10049);
#2377=VERTEX_POINT('',#10051);
#2378=VERTEX_POINT('',#10055);
#2379=VERTEX_POINT('',#10057);
#2380=VERTEX_POINT('',#10064);
#2381=VERTEX_POINT('',#10067);
#2382=VERTEX_POINT('',#10068);
#2383=VERTEX_POINT('',#10070);
#2384=VERTEX_POINT('',#10072);
#2385=VERTEX_POINT('',#10076);
#2386=VERTEX_POINT('',#10078);
#2387=VERTEX_POINT('',#10082);
#2388=VERTEX_POINT('',#10084);
#2389=VERTEX_POINT('',#10088);
#2390=VERTEX_POINT('',#10090);
#2391=VERTEX_POINT('',#10094);
#2392=VERTEX_POINT('',#10096);
#2393=VERTEX_POINT('',#10104);
#2394=VERTEX_POINT('',#10107);
#2395=VERTEX_POINT('',#10119);
#2396=VERTEX_POINT('',#10120);
#2397=VERTEX_POINT('',#10124);
#2398=VERTEX_POINT('',#10125);
#2399=VERTEX_POINT('',#10129);
#2400=VERTEX_POINT('',#10131);
#2401=VERTEX_POINT('',#10135);
#2402=VERTEX_POINT('',#10137);
#2403=VERTEX_POINT('',#10141);
#2404=VERTEX_POINT('',#10143);
#2405=VERTEX_POINT('',#10146);
#2406=VERTEX_POINT('',#10148);
#2407=VERTEX_POINT('',#10151);
#2408=VERTEX_POINT('',#10154);
#2409=VERTEX_POINT('',#10156);
#2410=VERTEX_POINT('',#10158);
#2411=VERTEX_POINT('',#10160);
#2412=VERTEX_POINT('',#10162);
#2413=VERTEX_POINT('',#10164);
#2414=VERTEX_POINT('',#10168);
#2415=VERTEX_POINT('',#10170);
#2416=VERTEX_POINT('',#10174);
#2417=VERTEX_POINT('',#10176);
#2418=VERTEX_POINT('',#10180);
#2419=VERTEX_POINT('',#10181);
#2420=VERTEX_POINT('',#10188);
#2421=VERTEX_POINT('',#10192);
#2422=VERTEX_POINT('',#10194);
#2423=VERTEX_POINT('',#10196);
#2424=VERTEX_POINT('',#10206);
#2425=VERTEX_POINT('',#10213);
#2426=VERTEX_POINT('',#10215);
#2427=VERTEX_POINT('',#10220);
#2428=VERTEX_POINT('',#10222);
#2429=VERTEX_POINT('',#10225);
#2430=VERTEX_POINT('',#10230);
#2431=VERTEX_POINT('',#10236);
#2432=VERTEX_POINT('',#10238);
#2433=VERTEX_POINT('',#10242);
#2434=VERTEX_POINT('',#10244);
#2435=VERTEX_POINT('',#10251);
#2436=VERTEX_POINT('',#10253);
#2437=VERTEX_POINT('',#10257);
#2438=VERTEX_POINT('',#10259);
#2439=VERTEX_POINT('',#10266);
#2440=VERTEX_POINT('',#10268);
#2441=VERTEX_POINT('',#10272);
#2442=VERTEX_POINT('',#10274);
#2443=VERTEX_POINT('',#10281);
#2444=VERTEX_POINT('',#10282);
#2445=VERTEX_POINT('',#10284);
#2446=VERTEX_POINT('',#10286);
#2447=VERTEX_POINT('',#10290);
#2448=VERTEX_POINT('',#10292);
#2449=VERTEX_POINT('',#10296);
#2450=VERTEX_POINT('',#10298);
#2451=VERTEX_POINT('',#10302);
#2452=VERTEX_POINT('',#10304);
#2453=VERTEX_POINT('',#10308);
#2454=VERTEX_POINT('',#10310);
#2455=VERTEX_POINT('',#10319);
#2456=VERTEX_POINT('',#10322);
#2457=VERTEX_POINT('',#10325);
#2458=VERTEX_POINT('',#10329);
#2459=VERTEX_POINT('',#10333);
#2460=VERTEX_POINT('',#10337);
#2461=VERTEX_POINT('',#10340);
#2462=VERTEX_POINT('',#10355);
#2463=VERTEX_POINT('',#10356);
#2464=VERTEX_POINT('',#10359);
#2465=VERTEX_POINT('',#10361);
#2466=VERTEX_POINT('',#10365);
#2467=VERTEX_POINT('',#10369);
#2468=VERTEX_POINT('',#10371);
#2469=VERTEX_POINT('',#10375);
#2470=VERTEX_POINT('',#10380);
#2471=VERTEX_POINT('',#10384);
#2472=VERTEX_POINT('',#10390);
#2473=VERTEX_POINT('',#10391);
#2474=VERTEX_POINT('',#10394);
#2475=VERTEX_POINT('',#10396);
#2476=VERTEX_POINT('',#10400);
#2477=VERTEX_POINT('',#10404);
#2478=VERTEX_POINT('',#10406);
#2479=VERTEX_POINT('',#10409);
#2480=VERTEX_POINT('',#10413);
#2481=VERTEX_POINT('',#10417);
#2482=VERTEX_POINT('',#10425);
#2483=VERTEX_POINT('',#10426);
#2484=VERTEX_POINT('',#10429);
#2485=VERTEX_POINT('',#10430);
#2486=VERTEX_POINT('',#10433);
#2487=VERTEX_POINT('',#10434);
#2488=VERTEX_POINT('',#10437);
#2489=VERTEX_POINT('',#10438);
#2490=VERTEX_POINT('',#10441);
#2491=VERTEX_POINT('',#10442);
#2492=VERTEX_POINT('',#10445);
#2493=VERTEX_POINT('',#10446);
#2494=VERTEX_POINT('',#10449);
#2495=VERTEX_POINT('',#10450);
#2496=VERTEX_POINT('',#10453);
#2497=VERTEX_POINT('',#10454);
#2498=VERTEX_POINT('',#10458);
#2499=VERTEX_POINT('',#10459);
#2500=VERTEX_POINT('',#10482);
#2501=VERTEX_POINT('',#10484);
#2502=VERTEX_POINT('',#10509);
#2503=VERTEX_POINT('',#10511);
#2504=VERTEX_POINT('',#10534);
#2505=VERTEX_POINT('',#10536);
#2506=VERTEX_POINT('',#10559);
#2507=VERTEX_POINT('',#10561);
#2508=VERTEX_POINT('',#10574);
#2509=VERTEX_POINT('',#10577);
#2510=VERTEX_POINT('',#10590);
#2511=VERTEX_POINT('',#10592);
#2512=VERTEX_POINT('',#10615);
#2513=VERTEX_POINT('',#10617);
#2514=VERTEX_POINT('',#10640);
#2515=VERTEX_POINT('',#10642);
#2516=VERTEX_POINT('',#10665);
#2517=VERTEX_POINT('',#10667);
#2518=VERTEX_POINT('',#10692);
#2519=VERTEX_POINT('',#10696);
#2520=VERTEX_POINT('',#10721);
#2521=VERTEX_POINT('',#10725);
#2522=VERTEX_POINT('',#10750);
#2523=VERTEX_POINT('',#10754);
#2524=VERTEX_POINT('',#10755);
#2525=VERTEX_POINT('',#10782);
#2526=VERTEX_POINT('',#10786);
#2527=VERTEX_POINT('',#10811);
#2528=VERTEX_POINT('',#10815);
#2529=VERTEX_POINT('',#10840);
#2530=VERTEX_POINT('',#10844);
#2531=VERTEX_POINT('',#10869);
#2532=VERTEX_POINT('',#10872);
#2533=VERTEX_POINT('',#10874);
#2534=VERTEX_POINT('',#10906);
#2535=VERTEX_POINT('',#10908);
#2536=VERTEX_POINT('',#10911);
#2537=VERTEX_POINT('',#10915);
#2538=VERTEX_POINT('',#10920);
#2539=VERTEX_POINT('',#10922);
#2540=VERTEX_POINT('',#10925);
#2541=VERTEX_POINT('',#10929);
#2542=EDGE_CURVE('',#2138,#2138,#1847,.T.);
#2543=EDGE_CURVE('',#2138,#2139,#1343,.T.);
#2544=EDGE_CURVE('',#2139,#2139,#1848,.T.);
#2545=EDGE_CURVE('',#2140,#2140,#1849,.T.);
#2546=EDGE_CURVE('',#2140,#2141,#1344,.T.);
#2547=EDGE_CURVE('',#2141,#2141,#1850,.T.);
#2548=EDGE_CURVE('',#2142,#2142,#1851,.T.);
#2549=EDGE_CURVE('',#2142,#2143,#1345,.T.);
#2550=EDGE_CURVE('',#2143,#2143,#1852,.T.);
#2551=EDGE_CURVE('',#2144,#2144,#1853,.T.);
#2552=EDGE_CURVE('',#2144,#2145,#1346,.T.);
#2553=EDGE_CURVE('',#2145,#2145,#1854,.T.);
#2554=EDGE_CURVE('',#2146,#2146,#1855,.T.);
#2555=EDGE_CURVE('',#2146,#2147,#1347,.T.);
#2556=EDGE_CURVE('',#2147,#2147,#1856,.T.);
#2557=EDGE_CURVE('',#2148,#2148,#1857,.T.);
#2558=EDGE_CURVE('',#2148,#2149,#1348,.T.);
#2559=EDGE_CURVE('',#2149,#2149,#1858,.T.);
#2560=EDGE_CURVE('',#2150,#2151,#1349,.T.);
#2561=EDGE_CURVE('',#2151,#2152,#1350,.T.);
#2562=EDGE_CURVE('',#2153,#2152,#1351,.T.);
#2563=EDGE_CURVE('',#2150,#2153,#1352,.T.);
#2564=EDGE_CURVE('',#2154,#2150,#1353,.T.);
#2565=EDGE_CURVE('',#2155,#2153,#1354,.T.);
#2566=EDGE_CURVE('',#2154,#2155,#1355,.T.);
#2567=EDGE_CURVE('',#2156,#2154,#1356,.T.);
#2568=EDGE_CURVE('',#2157,#2155,#1357,.T.);
#2569=EDGE_CURVE('',#2156,#2157,#1358,.T.);
#2570=EDGE_CURVE('',#2151,#2156,#1359,.T.);
#2571=EDGE_CURVE('',#2152,#2157,#1360,.T.);
#2572=EDGE_CURVE('',#2158,#2159,#1361,.T.);
#2573=EDGE_CURVE('',#2159,#2160,#1362,.T.);
#2574=EDGE_CURVE('',#2160,#2161,#1363,.T.);
#2575=EDGE_CURVE('',#2161,#2158,#1364,.T.);
#2576=EDGE_CURVE('',#2162,#2162,#1859,.T.);
#2577=EDGE_CURVE('',#2163,#2163,#1860,.T.);
#2578=EDGE_CURVE('',#2164,#2165,#1365,.T.);
#2579=EDGE_CURVE('',#2165,#2158,#1366,.T.);
#2580=EDGE_CURVE('',#2164,#2161,#1367,.T.);
#2581=EDGE_CURVE('',#2166,#2167,#1368,.T.);
#2582=EDGE_CURVE('',#2167,#2160,#1369,.T.);
#2583=EDGE_CURVE('',#2166,#2159,#1370,.T.);
#2584=EDGE_CURVE('',#2168,#2168,#1861,.T.);
#2585=EDGE_CURVE('',#2168,#2169,#1371,.T.);
#2586=EDGE_CURVE('',#2170,#2169,#241,.T.);
#2587=EDGE_CURVE('',#2169,#2170,#242,.T.);
#2588=EDGE_CURVE('',#2171,#2172,#243,.T.);
#2589=EDGE_CURVE('',#2172,#2171,#244,.T.);
#2590=EDGE_CURVE('',#2172,#2173,#1372,.T.);
#2591=EDGE_CURVE('',#2173,#2173,#1862,.T.);
#2592=EDGE_CURVE('',#2174,#2174,#1863,.T.);
#2593=EDGE_CURVE('',#2174,#2175,#1373,.T.);
#2594=EDGE_CURVE('',#2176,#2175,#245,.T.);
#2595=EDGE_CURVE('',#2175,#2176,#246,.T.);
#2596=EDGE_CURVE('',#2177,#2178,#247,.T.);
#2597=EDGE_CURVE('',#2178,#2177,#248,.T.);
#2598=EDGE_CURVE('',#2178,#2179,#1374,.T.);
#2599=EDGE_CURVE('',#2179,#2179,#1864,.T.);
#2600=EDGE_CURVE('',#2180,#2180,#1865,.T.);
#2601=EDGE_CURVE('',#2180,#2181,#1375,.T.);
#2602=EDGE_CURVE('',#2182,#2181,#249,.T.);
#2603=EDGE_CURVE('',#2181,#2182,#250,.T.);
#2604=EDGE_CURVE('',#2183,#2184,#251,.T.);
#2605=EDGE_CURVE('',#2184,#2183,#252,.T.);
#2606=EDGE_CURVE('',#2184,#2185,#1376,.T.);
#2607=EDGE_CURVE('',#2185,#2185,#1866,.T.);
#2608=EDGE_CURVE('',#2186,#2186,#1867,.T.);
#2609=EDGE_CURVE('',#2186,#2187,#1377,.T.);
#2610=EDGE_CURVE('',#2188,#2187,#253,.T.);
#2611=EDGE_CURVE('',#2187,#2188,#254,.T.);
#2612=EDGE_CURVE('',#2189,#2190,#255,.T.);
#2613=EDGE_CURVE('',#2190,#2189,#256,.T.);
#2614=EDGE_CURVE('',#2190,#2191,#1378,.T.);
#2615=EDGE_CURVE('',#2191,#2191,#1868,.T.);
#2616=EDGE_CURVE('',#2192,#2192,#1869,.T.);
#2617=EDGE_CURVE('',#2192,#2162,#1379,.T.);
#2618=EDGE_CURVE('',#2193,#2193,#257,.T.);
#2619=EDGE_CURVE('',#2194,#2194,#1870,.T.);
#2620=EDGE_CURVE('',#2195,#2195,#1871,.T.);
#2621=EDGE_CURVE('',#2195,#2194,#1380,.T.);
#2622=EDGE_CURVE('',#2196,#2196,#1872,.T.);
#2623=EDGE_CURVE('',#2196,#2163,#1381,.T.);
#2624=EDGE_CURVE('',#2197,#2197,#258,.T.);
#2625=EDGE_CURVE('',#2198,#2198,#1873,.T.);
#2626=EDGE_CURVE('',#2199,#2199,#1874,.T.);
#2627=EDGE_CURVE('',#2199,#2198,#1382,.T.);
#2628=EDGE_CURVE('',#2200,#2200,#1875,.T.);
#2629=EDGE_CURVE('',#2200,#2201,#1383,.T.);
#2630=EDGE_CURVE('',#2201,#2201,#1876,.T.);
#2631=EDGE_CURVE('',#2164,#2167,#1384,.T.);
#2632=EDGE_CURVE('',#2165,#2166,#1385,.T.);
#2633=EDGE_CURVE('',#2202,#2203,#1386,.T.);
#2634=EDGE_CURVE('',#2204,#2202,#1877,.T.);
#2635=EDGE_CURVE('',#2205,#2204,#1387,.T.);
#2636=EDGE_CURVE('',#2203,#2205,#1878,.T.);
#2637=EDGE_CURVE('',#2206,#2207,#1388,.T.);
#2638=EDGE_CURVE('',#2208,#2206,#1879,.T.);
#2639=EDGE_CURVE('',#2209,#2208,#1389,.T.);
#2640=EDGE_CURVE('',#2207,#2209,#1880,.T.);
#2641=EDGE_CURVE('',#2210,#2211,#1390,.T.);
#2642=EDGE_CURVE('',#2212,#2210,#1881,.T.);
#2643=EDGE_CURVE('',#2213,#2212,#1391,.T.);
#2644=EDGE_CURVE('',#2211,#2213,#1882,.T.);
#2645=EDGE_CURVE('',#2214,#2215,#1392,.T.);
#2646=EDGE_CURVE('',#2216,#2214,#1883,.T.);
#2647=EDGE_CURVE('',#2217,#2216,#1393,.T.);
#2648=EDGE_CURVE('',#2215,#2217,#1884,.T.);
#2649=EDGE_CURVE('',#2212,#2202,#1885,.T.);
#2650=EDGE_CURVE('',#2208,#2210,#1886,.T.);
#2651=EDGE_CURVE('',#2216,#2206,#1887,.T.);
#2652=EDGE_CURVE('',#2204,#2214,#1888,.T.);
#2653=EDGE_CURVE('',#2218,#2218,#1889,.T.);
#2654=EDGE_CURVE('',#2217,#2207,#1890,.T.);
#2655=EDGE_CURVE('',#2209,#2211,#1891,.T.);
#2656=EDGE_CURVE('',#2213,#2203,#1892,.T.);
#2657=EDGE_CURVE('',#2205,#2215,#1893,.T.);
#2658=EDGE_CURVE('',#2219,#2219,#1894,.T.);
#2659=EDGE_CURVE('',#2219,#2218,#1394,.T.);
#2660=EDGE_CURVE('',#2220,#2221,#1395,.T.);
#2661=EDGE_CURVE('',#2222,#2220,#1895,.T.);
#2662=EDGE_CURVE('',#2223,#2222,#1396,.T.);
#2663=EDGE_CURVE('',#2221,#2223,#1896,.T.);
#2664=EDGE_CURVE('',#2224,#2225,#1397,.T.);
#2665=EDGE_CURVE('',#2226,#2224,#1897,.T.);
#2666=EDGE_CURVE('',#2227,#2226,#1398,.T.);
#2667=EDGE_CURVE('',#2225,#2227,#1898,.T.);
#2668=EDGE_CURVE('',#2228,#2229,#1399,.T.);
#2669=EDGE_CURVE('',#2230,#2228,#1899,.T.);
#2670=EDGE_CURVE('',#2231,#2230,#1400,.T.);
#2671=EDGE_CURVE('',#2229,#2231,#1900,.T.);
#2672=EDGE_CURVE('',#2232,#2233,#1401,.T.);
#2673=EDGE_CURVE('',#2234,#2232,#1901,.T.);
#2674=EDGE_CURVE('',#2235,#2234,#1402,.T.);
#2675=EDGE_CURVE('',#2233,#2235,#1902,.T.);
#2676=EDGE_CURVE('',#2230,#2220,#1903,.T.);
#2677=EDGE_CURVE('',#2226,#2228,#1904,.T.);
#2678=EDGE_CURVE('',#2234,#2224,#1905,.T.);
#2679=EDGE_CURVE('',#2222,#2232,#1906,.T.);
#2680=EDGE_CURVE('',#2236,#2236,#1907,.T.);
#2681=EDGE_CURVE('',#2235,#2225,#1908,.T.);
#2682=EDGE_CURVE('',#2227,#2229,#1909,.T.);
#2683=EDGE_CURVE('',#2231,#2221,#1910,.T.);
#2684=EDGE_CURVE('',#2223,#2233,#1911,.T.);
#2685=EDGE_CURVE('',#2237,#2237,#1912,.T.);
#2686=EDGE_CURVE('',#2237,#2236,#1403,.T.);
#2687=EDGE_CURVE('',#2238,#2238,#1913,.T.);
#2688=EDGE_CURVE('',#2238,#2239,#259,.T.);
#2689=EDGE_CURVE('',#2239,#2239,#1914,.T.);
#2690=EDGE_CURVE('',#2240,#2241,#260,.T.);
#2691=EDGE_CURVE('',#2241,#2240,#261,.T.);
#2692=EDGE_CURVE('',#2241,#2242,#1404,.T.);
#2693=EDGE_CURVE('',#2243,#2242,#262,.T.);
#2694=EDGE_CURVE('',#2242,#2243,#263,.T.);
#2695=EDGE_CURVE('',#2244,#2244,#1915,.T.);
#2696=EDGE_CURVE('',#2244,#2245,#1405,.T.);
#2697=EDGE_CURVE('',#2245,#2245,#1916,.T.);
#2698=EDGE_CURVE('',#2246,#2246,#1917,.T.);
#2699=EDGE_CURVE('',#2246,#2247,#1406,.T.);
#2700=EDGE_CURVE('',#2247,#2247,#1918,.T.);
#2701=EDGE_CURVE('',#2248,#2248,#1919,.T.);
#2702=EDGE_CURVE('',#2248,#2249,#1407,.T.);
#2703=EDGE_CURVE('',#2249,#2249,#1920,.T.);
#2704=EDGE_CURVE('',#2250,#2250,#1921,.T.);
#2705=EDGE_CURVE('',#2250,#2251,#1408,.T.);
#2706=EDGE_CURVE('',#2251,#2251,#1922,.T.);
#2707=EDGE_CURVE('',#2252,#2253,#1923,.T.);
#2708=EDGE_CURVE('',#2253,#2252,#1924,.T.);
#2709=EDGE_CURVE('',#2254,#2252,#1409,.T.);
#2710=EDGE_CURVE('',#2255,#2254,#1925,.T.);
#2711=EDGE_CURVE('',#2253,#2255,#1410,.T.);
#2712=EDGE_CURVE('',#2256,#2257,#1411,.T.);
#2713=EDGE_CURVE('',#2256,#2258,#1926,.T.);
#2714=EDGE_CURVE('',#2259,#2258,#1412,.T.);
#2715=EDGE_CURVE('',#2257,#2259,#1927,.T.);
#2716=EDGE_CURVE('',#2258,#2256,#1928,.T.);
#2717=EDGE_CURVE('',#2260,#2261,#1413,.T.);
#2718=EDGE_CURVE('',#2260,#2262,#1929,.T.);
#2719=EDGE_CURVE('',#2263,#2262,#1414,.T.);
#2720=EDGE_CURVE('',#2261,#2263,#1930,.T.);
#2721=EDGE_CURVE('',#2262,#2260,#1931,.T.);
#2722=EDGE_CURVE('',#2264,#2265,#1415,.T.);
#2723=EDGE_CURVE('',#2264,#2266,#1932,.T.);
#2724=EDGE_CURVE('',#2267,#2266,#1416,.T.);
#2725=EDGE_CURVE('',#2265,#2267,#1933,.T.);
#2726=EDGE_CURVE('',#2266,#2264,#1934,.T.);
#2727=EDGE_CURVE('',#2268,#2268,#1935,.T.);
#2728=EDGE_CURVE('',#2268,#2269,#1417,.T.);
#2729=EDGE_CURVE('',#2269,#2254,#1936,.T.);
#2730=EDGE_CURVE('',#2255,#2267,#1937,.T.);
#2731=EDGE_CURVE('',#2265,#2263,#1938,.T.);
#2732=EDGE_CURVE('',#2261,#2259,#1939,.T.);
#2733=EDGE_CURVE('',#2257,#2269,#1940,.T.);
#2734=EDGE_CURVE('',#2270,#2270,#1941,.T.);
#2735=EDGE_CURVE('',#2271,#2271,#1942,.T.);
#2736=EDGE_CURVE('',#2272,#2272,#1943,.T.);
#2737=EDGE_CURVE('',#2273,#2273,#1944,.T.);
#2738=EDGE_CURVE('',#2274,#2274,#1945,.T.);
#2739=EDGE_CURVE('',#2275,#2275,#1946,.T.);
#2740=EDGE_CURVE('',#2275,#2271,#1418,.T.);
#2741=EDGE_CURVE('',#2276,#2276,#1947,.T.);
#2742=EDGE_CURVE('',#2276,#2274,#1419,.T.);
#2743=EDGE_CURVE('',#2277,#2277,#1948,.T.);
#2744=EDGE_CURVE('',#2277,#2272,#1420,.T.);
#2745=EDGE_CURVE('',#2278,#2278,#1949,.T.);
#2746=EDGE_CURVE('',#2278,#2273,#1421,.T.);
#2747=EDGE_CURVE('',#2279,#2279,#1950,.T.);
#2748=EDGE_CURVE('',#2279,#2280,#1422,.T.);
#2749=EDGE_CURVE('',#2280,#2280,#1951,.T.);
#2750=EDGE_CURVE('',#2281,#2281,#1952,.T.);
#2751=EDGE_CURVE('',#2270,#2282,#1423,.T.);
#2752=EDGE_CURVE('',#2282,#2282,#1953,.T.);
#2753=EDGE_CURVE('',#2281,#2283,#1424,.T.);
#2754=EDGE_CURVE('',#2283,#2283,#1954,.T.);
#2755=EDGE_CURVE('',#2284,#2284,#1955,.T.);
#2756=EDGE_CURVE('',#2284,#2285,#1425,.T.);
#2757=EDGE_CURVE('',#2285,#2285,#1956,.T.);
#2758=EDGE_CURVE('',#2286,#2286,#1957,.T.);
#2759=EDGE_CURVE('',#2287,#2287,#1958,.T.);
#2760=EDGE_CURVE('',#2287,#2288,#1426,.T.);
#2761=EDGE_CURVE('',#2288,#2288,#1959,.T.);
#2762=EDGE_CURVE('',#2289,#2289,#1960,.T.);
#2763=EDGE_CURVE('',#2290,#2290,#1961,.T.);
#2764=EDGE_CURVE('',#2290,#2291,#1427,.T.);
#2765=EDGE_CURVE('',#2291,#2291,#1962,.T.);
#2766=EDGE_CURVE('',#2292,#2292,#1963,.T.);
#2767=EDGE_CURVE('',#2293,#2293,#1964,.T.);
#2768=EDGE_CURVE('',#2293,#2294,#1428,.T.);
#2769=EDGE_CURVE('',#2294,#2294,#1965,.T.);
#2770=EDGE_CURVE('',#2295,#2295,#1966,.T.);
#2771=EDGE_CURVE('',#2296,#2296,#1967,.T.);
#2772=EDGE_CURVE('',#2296,#2286,#1429,.T.);
#2773=EDGE_CURVE('',#2297,#2297,#1968,.T.);
#2774=EDGE_CURVE('',#2297,#2289,#1430,.T.);
#2775=EDGE_CURVE('',#2298,#2298,#1969,.T.);
#2776=EDGE_CURVE('',#2298,#2292,#1431,.T.);
#2777=EDGE_CURVE('',#2299,#2299,#1970,.T.);
#2778=EDGE_CURVE('',#2299,#2295,#1432,.T.);
#2779=EDGE_CURVE('',#2300,#2300,#1971,.T.);
#2780=EDGE_CURVE('',#2300,#2301,#1433,.T.);
#2781=EDGE_CURVE('',#2301,#2301,#1972,.T.);
#2782=EDGE_CURVE('',#2302,#2302,#1973,.T.);
#2783=EDGE_CURVE('',#2303,#2303,#1974,.T.);
#2784=EDGE_CURVE('',#2303,#2302,#1434,.T.);
#2785=EDGE_CURVE('',#2304,#2304,#1975,.T.);
#2786=EDGE_CURVE('',#2304,#2305,#1435,.T.);
#2787=EDGE_CURVE('',#2305,#2305,#1976,.T.);
#2788=EDGE_CURVE('',#2306,#2307,#1977,.T.);
#2789=EDGE_CURVE('',#2308,#2306,#1436,.T.);
#2790=EDGE_CURVE('',#2309,#2308,#1437,.T.);
#2791=EDGE_CURVE('',#2307,#2309,#1438,.T.);
#2792=EDGE_CURVE('',#2307,#2310,#1439,.T.);
#2793=EDGE_CURVE('',#2311,#2309,#1440,.T.);
#2794=EDGE_CURVE('',#2311,#2310,#1441,.T.);
#2795=EDGE_CURVE('',#2310,#2312,#1978,.T.);
#2796=EDGE_CURVE('',#2313,#2311,#1442,.T.);
#2797=EDGE_CURVE('',#2312,#2313,#1443,.T.);
#2798=EDGE_CURVE('',#2312,#2306,#1444,.T.);
#2799=EDGE_CURVE('',#2313,#2308,#1445,.T.);
#2800=EDGE_CURVE('',#2314,#2314,#1979,.T.);
#2801=EDGE_CURVE('',#2315,#2315,#1980,.T.);
#2802=EDGE_CURVE('',#2316,#2316,#1981,.T.);
#2803=EDGE_CURVE('',#2316,#2314,#1446,.T.);
#2804=EDGE_CURVE('',#2317,#2317,#1982,.T.);
#2805=EDGE_CURVE('',#2318,#2318,#1983,.T.);
#2806=EDGE_CURVE('',#2318,#2317,#1447,.T.);
#2807=EDGE_CURVE('',#2319,#2319,#1984,.T.);
#2808=EDGE_CURVE('',#2320,#2320,#1985,.T.);
#2809=EDGE_CURVE('',#2320,#2319,#1448,.T.);
#2810=EDGE_CURVE('',#2321,#2321,#1986,.T.);
#2811=EDGE_CURVE('',#2322,#2322,#1987,.T.);
#2812=EDGE_CURVE('',#2322,#2321,#1449,.T.);
#2813=EDGE_CURVE('',#2323,#2323,#1988,.T.);
#2814=EDGE_CURVE('',#2324,#2324,#1989,.T.);
#2815=EDGE_CURVE('',#2324,#2323,#1450,.T.);
#2816=EDGE_CURVE('',#2325,#2325,#1990,.T.);
#2817=EDGE_CURVE('',#2325,#2315,#1451,.T.);
#2818=EDGE_CURVE('',#2326,#2327,#1991,.T.);
#2819=EDGE_CURVE('',#2328,#2326,#1452,.T.);
#2820=EDGE_CURVE('',#2329,#2328,#1992,.T.);
#2821=EDGE_CURVE('',#2327,#2329,#1453,.T.);
#2822=EDGE_CURVE('',#2327,#2330,#1454,.T.);
#2823=EDGE_CURVE('',#2331,#2329,#1455,.T.);
#2824=EDGE_CURVE('',#2331,#2330,#1456,.T.);
#2825=EDGE_CURVE('',#2330,#2332,#1993,.T.);
#2826=EDGE_CURVE('',#2333,#2331,#1994,.T.);
#2827=EDGE_CURVE('',#2332,#2333,#1457,.T.);
#2828=EDGE_CURVE('',#2332,#2326,#1458,.T.);
#2829=EDGE_CURVE('',#2328,#2333,#1459,.T.);
#2830=EDGE_CURVE('',#2334,#2334,#1995,.T.);
#2831=EDGE_CURVE('',#2335,#2335,#1996,.T.);
#2832=EDGE_CURVE('',#2336,#2336,#1997,.T.);
#2833=EDGE_CURVE('',#2336,#2334,#1460,.T.);
#2834=EDGE_CURVE('',#2337,#2337,#1998,.T.);
#2835=EDGE_CURVE('',#2337,#2335,#1461,.T.);
#2836=EDGE_CURVE('',#2338,#2339,#1462,.T.);
#2837=EDGE_CURVE('',#2339,#2340,#1463,.T.);
#2838=EDGE_CURVE('',#2340,#2341,#1464,.T.);
#2839=EDGE_CURVE('',#2338,#2341,#1465,.T.);
#2840=EDGE_CURVE('',#2339,#2342,#1466,.T.);
#2841=EDGE_CURVE('',#2342,#2343,#1467,.T.);
#2842=EDGE_CURVE('',#2343,#2340,#1468,.T.);
#2843=EDGE_CURVE('',#2342,#2344,#1469,.T.);
#2844=EDGE_CURVE('',#2344,#2345,#1470,.T.);
#2845=EDGE_CURVE('',#2345,#2343,#1471,.T.);
#2846=EDGE_CURVE('',#2344,#2346,#1472,.T.);
#2847=EDGE_CURVE('',#2346,#2347,#1473,.T.);
#2848=EDGE_CURVE('',#2347,#2345,#1474,.T.);
#2849=EDGE_CURVE('',#2346,#2348,#1475,.T.);
#2850=EDGE_CURVE('',#2348,#2349,#1476,.T.);
#2851=EDGE_CURVE('',#2349,#2347,#1477,.T.);
#2852=EDGE_CURVE('',#2348,#2338,#1478,.T.);
#2853=EDGE_CURVE('',#2341,#2349,#1479,.T.);
#2854=EDGE_CURVE('',#2350,#2350,#1999,.T.);
#2855=EDGE_CURVE('',#2351,#2351,#2000,.T.);
#2856=EDGE_CURVE('',#2352,#2352,#2001,.T.);
#2857=EDGE_CURVE('',#2352,#2351,#1480,.T.);
#2858=EDGE_CURVE('',#2353,#2353,#2002,.T.);
#2859=EDGE_CURVE('',#2353,#2352,#1481,.T.);
#2860=EDGE_CURVE('',#2354,#2354,#2003,.T.);
#2861=EDGE_CURVE('',#2354,#2353,#1482,.T.);
#2862=EDGE_CURVE('',#2355,#2355,#2004,.T.);
#2863=EDGE_CURVE('',#2356,#2356,#2005,.F.);
#2864=EDGE_CURVE('',#2356,#2355,#1483,.T.);
#2865=EDGE_CURVE('',#2350,#2356,#1484,.T.);
#2866=EDGE_CURVE('',#2357,#2357,#2006,.T.);
#2867=EDGE_CURVE('',#2358,#2358,#2007,.T.);
#2868=EDGE_CURVE('',#2359,#2359,#2008,.T.);
#2869=EDGE_CURVE('',#2360,#2360,#2009,.T.);
#2870=EDGE_CURVE('',#2357,#2359,#1485,.T.);
#2871=EDGE_CURVE('',#2361,#2361,#2010,.T.);
#2872=EDGE_CURVE('',#2362,#2362,#2011,.T.);
#2873=EDGE_CURVE('',#2360,#2361,#1486,.T.);
#2874=EDGE_CURVE('',#2362,#2363,#1487,.T.);
#2875=EDGE_CURVE('',#2363,#2363,#2012,.T.);
#2876=EDGE_CURVE('',#2364,#2364,#2013,.T.);
#2877=EDGE_CURVE('',#2364,#2358,#1488,.T.);
#2878=EDGE_CURVE('',#2365,#2365,#2014,.T.);
#2879=EDGE_CURVE('',#2365,#2366,#1489,.T.);
#2880=EDGE_CURVE('',#2366,#2366,#2015,.T.);
#2881=EDGE_CURVE('',#2367,#2367,#2016,.T.);
#2882=EDGE_CURVE('',#2367,#2368,#1490,.T.);
#2883=EDGE_CURVE('',#2368,#2368,#2017,.T.);
#2884=EDGE_CURVE('',#2369,#2370,#1491,.T.);
#2885=EDGE_CURVE('',#2369,#2370,#2018,.T.);
#2886=EDGE_CURVE('',#2371,#2369,#264,.T.);
#2887=EDGE_CURVE('',#2372,#2371,#2019,.T.);
#2888=EDGE_CURVE('',#2373,#2372,#265,.T.);
#2889=EDGE_CURVE('',#2373,#2374,#1492,.T.);
#2890=EDGE_CURVE('',#2375,#2374,#266,.T.);
#2891=EDGE_CURVE('',#2374,#2375,#267,.T.);
#2892=EDGE_CURVE('',#2370,#2373,#268,.T.);
#2893=EDGE_CURVE('',#2372,#2371,#1493,.T.);
#2894=EDGE_CURVE('',#2376,#2376,#2020,.T.);
#2895=EDGE_CURVE('',#2376,#2377,#1494,.T.);
#2896=EDGE_CURVE('',#2377,#2377,#2021,.T.);
#2897=EDGE_CURVE('',#2378,#2378,#2022,.T.);
#2898=EDGE_CURVE('',#2378,#2379,#1495,.T.);
#2899=EDGE_CURVE('',#2379,#2379,#2023,.T.);
#2900=EDGE_CURVE('',#2380,#2380,#2024,.T.);
#2901=EDGE_CURVE('',#2381,#2382,#1496,.T.);
#2902=EDGE_CURVE('',#2381,#2383,#1497,.T.);
#2903=EDGE_CURVE('',#2383,#2384,#1498,.T.);
#2904=EDGE_CURVE('',#2382,#2384,#1499,.T.);
#2905=EDGE_CURVE('',#2385,#2381,#1500,.T.);
#2906=EDGE_CURVE('',#2385,#2386,#1501,.T.);
#2907=EDGE_CURVE('',#2386,#2383,#1502,.T.);
#2908=EDGE_CURVE('',#2387,#2385,#1503,.T.);
#2909=EDGE_CURVE('',#2387,#2388,#1504,.T.);
#2910=EDGE_CURVE('',#2388,#2386,#1505,.T.);
#2911=EDGE_CURVE('',#2389,#2387,#1506,.T.);
#2912=EDGE_CURVE('',#2389,#2390,#1507,.T.);
#2913=EDGE_CURVE('',#2390,#2388,#1508,.T.);
#2914=EDGE_CURVE('',#2391,#2389,#1509,.T.);
#2915=EDGE_CURVE('',#2391,#2392,#1510,.T.);
#2916=EDGE_CURVE('',#2392,#2390,#1511,.T.);
#2917=EDGE_CURVE('',#2382,#2391,#1512,.T.);
#2918=EDGE_CURVE('',#2384,#2392,#1513,.T.);
#2919=EDGE_CURVE('',#2393,#2393,#2025,.T.);
#2920=EDGE_CURVE('',#2394,#2394,#2026,.T.);
#2921=EDGE_CURVE('',#2394,#2393,#1514,.T.);
#2922=EDGE_CURVE('',#2380,#2394,#1515,.T.);
#2923=EDGE_CURVE('',#2395,#2396,#1516,.T.);
#2924=EDGE_CURVE('',#2396,#2395,#2027,.T.);
#2925=EDGE_CURVE('',#2397,#2398,#1517,.T.);
#2926=EDGE_CURVE('',#2398,#2397,#2028,.T.);
#2927=EDGE_CURVE('',#2399,#2395,#1518,.T.);
#2928=EDGE_CURVE('',#2400,#2399,#2029,.T.);
#2929=EDGE_CURVE('',#2396,#2400,#1519,.T.);
#2930=EDGE_CURVE('',#2398,#2401,#1520,.T.);
#2931=EDGE_CURVE('',#2402,#2397,#1521,.T.);
#2932=EDGE_CURVE('',#2401,#2402,#2030,.T.);
#2933=EDGE_CURVE('',#2402,#2403,#1522,.T.);
#2934=EDGE_CURVE('',#2403,#2404,#1523,.T.);
#2935=EDGE_CURVE('',#2404,#2400,#1524,.T.);
#2936=EDGE_CURVE('',#2399,#2405,#1525,.T.);
#2937=EDGE_CURVE('',#2405,#2406,#1526,.T.);
#2938=EDGE_CURVE('',#2406,#2401,#1527,.T.);
#2939=EDGE_CURVE('',#2407,#2407,#2031,.T.);
#2940=EDGE_CURVE('',#2408,#2404,#1528,.T.);
#2941=EDGE_CURVE('',#2409,#2408,#1529,.T.);
#2942=EDGE_CURVE('',#2409,#2410,#1530,.T.);
#2943=EDGE_CURVE('',#2410,#2411,#1531,.T.);
#2944=EDGE_CURVE('',#2412,#2411,#1532,.T.);
#2945=EDGE_CURVE('',#2413,#2412,#1533,.T.);
#2946=EDGE_CURVE('',#2413,#2405,#1534,.T.);
#2947=EDGE_CURVE('',#2414,#2414,#2032,.T.);
#2948=EDGE_CURVE('',#2414,#2415,#1535,.T.);
#2949=EDGE_CURVE('',#2415,#2415,#2033,.T.);
#2950=EDGE_CURVE('',#2416,#2416,#2034,.T.);
#2951=EDGE_CURVE('',#2416,#2417,#1536,.T.);
#2952=EDGE_CURVE('',#2417,#2417,#2035,.T.);
#2953=EDGE_CURVE('',#2418,#2419,#1537,.T.);
#2954=EDGE_CURVE('',#2418,#2409,#2036,.T.);
#2955=EDGE_CURVE('',#2419,#2408,#2037,.T.);
#2956=EDGE_CURVE('',#2419,#2403,#1538,.T.);
#2957=EDGE_CURVE('',#2420,#2418,#1539,.T.);
#2958=EDGE_CURVE('',#2410,#2420,#1540,.T.);
#2959=EDGE_CURVE('',#2421,#2406,#1541,.T.);
#2960=EDGE_CURVE('',#2421,#2422,#1542,.T.);
#2961=EDGE_CURVE('',#2423,#2422,#1543,.T.);
#2962=EDGE_CURVE('',#2423,#2420,#1544,.T.);
#2963=EDGE_CURVE('',#2422,#2412,#2038,.T.);
#2964=EDGE_CURVE('',#2421,#2413,#2039,.T.);
#2965=EDGE_CURVE('',#2423,#2411,#1545,.T.);
#2966=EDGE_CURVE('',#2424,#2424,#2040,.T.);
#2967=EDGE_CURVE('',#2424,#2407,#1546,.T.);
#2968=EDGE_CURVE('',#2425,#2425,#2041,.T.);
#2969=EDGE_CURVE('',#2425,#2426,#1547,.T.);
#2970=EDGE_CURVE('',#2426,#2426,#2042,.T.);
#2971=EDGE_CURVE('',#2427,#2427,#2043,.T.);
#2972=EDGE_CURVE('',#2428,#2428,#2044,.T.);
#2973=EDGE_CURVE('',#2427,#2429,#1548,.T.);
#2974=EDGE_CURVE('',#2429,#2429,#2045,.T.);
#2975=EDGE_CURVE('',#2430,#2430,#2046,.T.);
#2976=EDGE_CURVE('',#2430,#2428,#1549,.T.);
#2977=EDGE_CURVE('',#2431,#2431,#2047,.T.);
#2978=EDGE_CURVE('',#2431,#2432,#1550,.T.);
#2979=EDGE_CURVE('',#2432,#2432,#2048,.T.);
#2980=EDGE_CURVE('',#2433,#2433,#2049,.T.);
#2981=EDGE_CURVE('',#2433,#2434,#1551,.T.);
#2982=EDGE_CURVE('',#2434,#2434,#2050,.T.);
#2983=EDGE_CURVE('',#2435,#2435,#2051,.T.);
#2984=EDGE_CURVE('',#2435,#2436,#1552,.T.);
#2985=EDGE_CURVE('',#2436,#2436,#2052,.T.);
#2986=EDGE_CURVE('',#2437,#2437,#2053,.T.);
#2987=EDGE_CURVE('',#2437,#2438,#1553,.T.);
#2988=EDGE_CURVE('',#2438,#2438,#2054,.T.);
#2989=EDGE_CURVE('',#2439,#2439,#2055,.T.);
#2990=EDGE_CURVE('',#2439,#2440,#1554,.T.);
#2991=EDGE_CURVE('',#2440,#2440,#2056,.T.);
#2992=EDGE_CURVE('',#2441,#2441,#2057,.T.);
#2993=EDGE_CURVE('',#2441,#2442,#1555,.T.);
#2994=EDGE_CURVE('',#2442,#2442,#2058,.T.);
#2995=EDGE_CURVE('',#2443,#2444,#1556,.T.);
#2996=EDGE_CURVE('',#2444,#2445,#1557,.T.);
#2997=EDGE_CURVE('',#2445,#2446,#1558,.T.);
#2998=EDGE_CURVE('',#2443,#2446,#1559,.T.);
#2999=EDGE_CURVE('',#2444,#2447,#1560,.T.);
#3000=EDGE_CURVE('',#2447,#2448,#1561,.T.);
#3001=EDGE_CURVE('',#2448,#2445,#1562,.T.);
#3002=EDGE_CURVE('',#2447,#2449,#1563,.T.);
#3003=EDGE_CURVE('',#2449,#2450,#1564,.T.);
#3004=EDGE_CURVE('',#2450,#2448,#1565,.T.);
#3005=EDGE_CURVE('',#2449,#2451,#1566,.T.);
#3006=EDGE_CURVE('',#2451,#2452,#1567,.T.);
#3007=EDGE_CURVE('',#2452,#2450,#1568,.T.);
#3008=EDGE_CURVE('',#2451,#2453,#1569,.T.);
#3009=EDGE_CURVE('',#2453,#2454,#1570,.T.);
#3010=EDGE_CURVE('',#2454,#2452,#1571,.T.);
#3011=EDGE_CURVE('',#2453,#2443,#1572,.T.);
#3012=EDGE_CURVE('',#2446,#2454,#1573,.T.);
#3013=EDGE_CURVE('',#2455,#2455,#2059,.T.);
#3014=EDGE_CURVE('',#2456,#2456,#2060,.T.);
#3015=EDGE_CURVE('',#2457,#2457,#2061,.T.);
#3016=EDGE_CURVE('',#2457,#2456,#1574,.T.);
#3017=EDGE_CURVE('',#2458,#2458,#2062,.T.);
#3018=EDGE_CURVE('',#2458,#2457,#1575,.T.);
#3019=EDGE_CURVE('',#2459,#2459,#2063,.T.);
#3020=EDGE_CURVE('',#2459,#2458,#1576,.T.);
#3021=EDGE_CURVE('',#2460,#2460,#2064,.T.);
#3022=EDGE_CURVE('',#2461,#2461,#2065,.F.);
#3023=EDGE_CURVE('',#2461,#2460,#1577,.T.);
#3024=EDGE_CURVE('',#2455,#2461,#1578,.T.);
#3025=EDGE_CURVE('',#2462,#2463,#2066,.T.);
#3026=EDGE_CURVE('',#2463,#2462,#2067,.T.);
#3027=EDGE_CURVE('',#2463,#2464,#2068,.T.);
#3028=EDGE_CURVE('',#2465,#2464,#2069,.T.);
#3029=EDGE_CURVE('',#2464,#2465,#2070,.T.);
#3030=EDGE_CURVE('',#2465,#2466,#1579,.T.);
#3031=EDGE_CURVE('',#2466,#2466,#2071,.T.);
#3032=EDGE_CURVE('',#2467,#2467,#2072,.T.);
#3033=EDGE_CURVE('',#2467,#2468,#1580,.T.);
#3034=EDGE_CURVE('',#2468,#2468,#2073,.T.);
#3035=EDGE_CURVE('',#2468,#2469,#1581,.T.);
#3036=EDGE_CURVE('',#2469,#2469,#2074,.T.);
#3037=EDGE_CURVE('',#2470,#2470,#2075,.T.);
#3038=EDGE_CURVE('',#2470,#2462,#1582,.T.);
#3039=EDGE_CURVE('',#2471,#2471,#2076,.T.);
#3040=EDGE_CURVE('',#2471,#2467,#1583,.T.);
#3041=EDGE_CURVE('',#2472,#2473,#2077,.T.);
#3042=EDGE_CURVE('',#2473,#2472,#2078,.T.);
#3043=EDGE_CURVE('',#2473,#2474,#2079,.T.);
#3044=EDGE_CURVE('',#2475,#2474,#2080,.T.);
#3045=EDGE_CURVE('',#2474,#2475,#2081,.T.);
#3046=EDGE_CURVE('',#2476,#2476,#2082,.T.);
#3047=EDGE_CURVE('',#2476,#2475,#1584,.T.);
#3048=EDGE_CURVE('',#2477,#2477,#2083,.T.);
#3049=EDGE_CURVE('',#2478,#2478,#2084,.T.);
#3050=EDGE_CURVE('',#2479,#2479,#2085,.T.);
#3051=EDGE_CURVE('',#2479,#2477,#1585,.T.);
#3052=EDGE_CURVE('',#2480,#2480,#2086,.T.);
#3053=EDGE_CURVE('',#2480,#2479,#1586,.T.);
#3054=EDGE_CURVE('',#2481,#2481,#2087,.T.);
#3055=EDGE_CURVE('',#2481,#2480,#1587,.T.);
#3056=EDGE_CURVE('',#2472,#2478,#1588,.T.);
#3057=EDGE_CURVE('',#2482,#2483,#2088,.T.);
#3058=EDGE_CURVE('',#2484,#2485,#2089,.T.);
#3059=EDGE_CURVE('',#2486,#2487,#2090,.T.);
#3060=EDGE_CURVE('',#2488,#2489,#2091,.T.);
#3061=EDGE_CURVE('',#2490,#2491,#2092,.T.);
#3062=EDGE_CURVE('',#2492,#2493,#2093,.T.);
#3063=EDGE_CURVE('',#2494,#2495,#2094,.T.);
#3064=EDGE_CURVE('',#2496,#2497,#2095,.T.);
#3065=EDGE_CURVE('',#2498,#2499,#269,.T.);
#3066=EDGE_CURVE('',#2500,#2498,#2096,.T.);
#3067=EDGE_CURVE('',#2501,#2500,#270,.T.);
#3068=EDGE_CURVE('',#2499,#2501,#2097,.T.);
#3069=EDGE_CURVE('',#2502,#2500,#2098,.T.);
#3070=EDGE_CURVE('',#2502,#2503,#271,.T.);
#3071=EDGE_CURVE('',#2504,#2503,#2099,.T.);
#3072=EDGE_CURVE('',#2504,#2505,#272,.T.);
#3073=EDGE_CURVE('',#2506,#2505,#2100,.T.);
#3074=EDGE_CURVE('',#2506,#2507,#273,.T.);
#3075=EDGE_CURVE('',#2507,#2508,#1589,.T.);
#3076=EDGE_CURVE('',#2508,#2508,#2101,.T.);
#3077=EDGE_CURVE('',#2507,#2509,#274,.T.);
#3078=EDGE_CURVE('',#2510,#2509,#2102,.T.);
#3079=EDGE_CURVE('',#2510,#2511,#275,.T.);
#3080=EDGE_CURVE('',#2512,#2511,#2103,.T.);
#3081=EDGE_CURVE('',#2512,#2513,#276,.T.);
#3082=EDGE_CURVE('',#2514,#2513,#2104,.T.);
#3083=EDGE_CURVE('',#2514,#2515,#277,.T.);
#3084=EDGE_CURVE('',#2516,#2515,#2105,.T.);
#3085=EDGE_CURVE('',#2516,#2517,#278,.T.);
#3086=EDGE_CURVE('',#2501,#2517,#2106,.T.);
#3087=EDGE_CURVE('',#2498,#2518,#2107,.T.);
#3088=EDGE_CURVE('',#2518,#2502,#2108,.T.);
#3089=EDGE_CURVE('',#2519,#2518,#279,.T.);
#3090=EDGE_CURVE('',#2503,#2519,#2109,.T.);
#3091=EDGE_CURVE('',#2519,#2520,#2110,.T.);
#3092=EDGE_CURVE('',#2520,#2504,#2111,.T.);
#3093=EDGE_CURVE('',#2521,#2520,#280,.T.);
#3094=EDGE_CURVE('',#2505,#2521,#2112,.T.);
#3095=EDGE_CURVE('',#2521,#2522,#2113,.T.);
#3096=EDGE_CURVE('',#2522,#2506,#2114,.T.);
#3097=EDGE_CURVE('',#2523,#2524,#281,.T.);
#3098=EDGE_CURVE('',#2509,#2523,#2115,.T.);
#3099=EDGE_CURVE('',#2524,#2522,#282,.T.);
#3100=EDGE_CURVE('',#2523,#2525,#2116,.T.);
#3101=EDGE_CURVE('',#2525,#2510,#2117,.T.);
#3102=EDGE_CURVE('',#2526,#2525,#283,.T.);
#3103=EDGE_CURVE('',#2511,#2526,#2118,.T.);
#3104=EDGE_CURVE('',#2526,#2527,#2119,.T.);
#3105=EDGE_CURVE('',#2527,#2512,#2120,.T.);
#3106=EDGE_CURVE('',#2528,#2527,#284,.T.);
#3107=EDGE_CURVE('',#2513,#2528,#2121,.T.);
#3108=EDGE_CURVE('',#2528,#2529,#2122,.T.);
#3109=EDGE_CURVE('',#2529,#2514,#2123,.T.);
#3110=EDGE_CURVE('',#2530,#2529,#285,.T.);
#3111=EDGE_CURVE('',#2515,#2530,#2124,.T.);
#3112=EDGE_CURVE('',#2531,#2531,#2125,.T.);
#3113=EDGE_CURVE('',#2531,#2524,#1590,.T.);
#3114=EDGE_CURVE('',#2532,#2499,#2126,.T.);
#3115=EDGE_CURVE('',#2532,#2533,#286,.T.);
#3116=EDGE_CURVE('',#2530,#2533,#2127,.T.);
#3117=EDGE_CURVE('',#2517,#2532,#2128,.T.);
#3118=EDGE_CURVE('',#2533,#2516,#2129,.T.);
#3119=EDGE_CURVE('',#2534,#2534,#2130,.T.);
#3120=EDGE_CURVE('',#2535,#2535,#2131,.T.);
#3121=EDGE_CURVE('',#2536,#2536,#2132,.T.);
#3122=EDGE_CURVE('',#2536,#2534,#1591,.T.);
#3123=EDGE_CURVE('',#2537,#2537,#2133,.T.);
#3124=EDGE_CURVE('',#2537,#2535,#1592,.T.);
#3125=EDGE_CURVE('',#2538,#2538,#2134,.T.);
#3126=EDGE_CURVE('',#2539,#2539,#2135,.T.);
#3127=EDGE_CURVE('',#2540,#2540,#2136,.T.);
#3128=EDGE_CURVE('',#2540,#2538,#1593,.T.);
#3129=EDGE_CURVE('',#2541,#2541,#2137,.T.);
#3130=EDGE_CURVE('',#2541,#2539,#1594,.T.);
#3131=ORIENTED_EDGE('',*,*,#2542,.F.);
#3132=ORIENTED_EDGE('',*,*,#2543,.T.);
#3133=ORIENTED_EDGE('',*,*,#2544,.F.);
#3134=ORIENTED_EDGE('',*,*,#2543,.F.);
#3135=ORIENTED_EDGE('',*,*,#2545,.F.);
#3136=ORIENTED_EDGE('',*,*,#2546,.T.);
#3137=ORIENTED_EDGE('',*,*,#2547,.F.);
#3138=ORIENTED_EDGE('',*,*,#2546,.F.);
#3139=ORIENTED_EDGE('',*,*,#2548,.F.);
#3140=ORIENTED_EDGE('',*,*,#2549,.T.);
#3141=ORIENTED_EDGE('',*,*,#2550,.F.);
#3142=ORIENTED_EDGE('',*,*,#2549,.F.);
#3143=ORIENTED_EDGE('',*,*,#2551,.F.);
#3144=ORIENTED_EDGE('',*,*,#2552,.T.);
#3145=ORIENTED_EDGE('',*,*,#2553,.F.);
#3146=ORIENTED_EDGE('',*,*,#2552,.F.);
#3147=ORIENTED_EDGE('',*,*,#2554,.F.);
#3148=ORIENTED_EDGE('',*,*,#2555,.T.);
#3149=ORIENTED_EDGE('',*,*,#2556,.F.);
#3150=ORIENTED_EDGE('',*,*,#2555,.F.);
#3151=ORIENTED_EDGE('',*,*,#2557,.F.);
#3152=ORIENTED_EDGE('',*,*,#2558,.T.);
#3153=ORIENTED_EDGE('',*,*,#2559,.F.);
#3154=ORIENTED_EDGE('',*,*,#2558,.F.);
#3155=ORIENTED_EDGE('',*,*,#2560,.T.);
#3156=ORIENTED_EDGE('',*,*,#2561,.T.);
#3157=ORIENTED_EDGE('',*,*,#2562,.F.);
#3158=ORIENTED_EDGE('',*,*,#2563,.F.);
#3159=ORIENTED_EDGE('',*,*,#2564,.T.);
#3160=ORIENTED_EDGE('',*,*,#2563,.T.);
#3161=ORIENTED_EDGE('',*,*,#2565,.F.);
#3162=ORIENTED_EDGE('',*,*,#2566,.F.);
#3163=ORIENTED_EDGE('',*,*,#2567,.T.);
#3164=ORIENTED_EDGE('',*,*,#2566,.T.);
#3165=ORIENTED_EDGE('',*,*,#2568,.F.);
#3166=ORIENTED_EDGE('',*,*,#2569,.F.);
#3167=ORIENTED_EDGE('',*,*,#2570,.T.);
#3168=ORIENTED_EDGE('',*,*,#2569,.T.);
#3169=ORIENTED_EDGE('',*,*,#2571,.F.);
#3170=ORIENTED_EDGE('',*,*,#2561,.F.);
#3171=ORIENTED_EDGE('',*,*,#2571,.T.);
#3172=ORIENTED_EDGE('',*,*,#2568,.T.);
#3173=ORIENTED_EDGE('',*,*,#2565,.T.);
#3174=ORIENTED_EDGE('',*,*,#2562,.T.);
#3175=ORIENTED_EDGE('',*,*,#2544,.T.);
#3176=ORIENTED_EDGE('',*,*,#2547,.T.);
#3177=ORIENTED_EDGE('',*,*,#2550,.T.);
#3178=ORIENTED_EDGE('',*,*,#2553,.T.);
#3179=ORIENTED_EDGE('',*,*,#2556,.T.);
#3180=ORIENTED_EDGE('',*,*,#2559,.T.);
#3181=ORIENTED_EDGE('',*,*,#2570,.F.);
#3182=ORIENTED_EDGE('',*,*,#2560,.F.);
#3183=ORIENTED_EDGE('',*,*,#2564,.F.);
#3184=ORIENTED_EDGE('',*,*,#2567,.F.);
#3185=ORIENTED_EDGE('',*,*,#2542,.T.);
#3186=ORIENTED_EDGE('',*,*,#2545,.T.);
#3187=ORIENTED_EDGE('',*,*,#2548,.T.);
#3188=ORIENTED_EDGE('',*,*,#2551,.T.);
#3189=ORIENTED_EDGE('',*,*,#2554,.T.);
#3190=ORIENTED_EDGE('',*,*,#2557,.T.);
#3191=ORIENTED_EDGE('',*,*,#2572,.T.);
#3192=ORIENTED_EDGE('',*,*,#2573,.T.);
#3193=ORIENTED_EDGE('',*,*,#2574,.T.);
#3194=ORIENTED_EDGE('',*,*,#2575,.T.);
#3195=ORIENTED_EDGE('',*,*,#2576,.T.);
#3196=ORIENTED_EDGE('',*,*,#2577,.T.);
#3197=ORIENTED_EDGE('',*,*,#2578,.T.);
#3198=ORIENTED_EDGE('',*,*,#2579,.T.);
#3199=ORIENTED_EDGE('',*,*,#2575,.F.);
#3200=ORIENTED_EDGE('',*,*,#2580,.F.);
#3201=ORIENTED_EDGE('',*,*,#2581,.T.);
#3202=ORIENTED_EDGE('',*,*,#2582,.T.);
#3203=ORIENTED_EDGE('',*,*,#2573,.F.);
#3204=ORIENTED_EDGE('',*,*,#2583,.F.);
#3205=ORIENTED_EDGE('',*,*,#2584,.F.);
#3206=ORIENTED_EDGE('',*,*,#2585,.T.);
#3207=ORIENTED_EDGE('',*,*,#2586,.F.);
#3208=ORIENTED_EDGE('',*,*,#2587,.F.);
#3209=ORIENTED_EDGE('',*,*,#2585,.F.);
#3210=ORIENTED_EDGE('',*,*,#2588,.F.);
#3211=ORIENTED_EDGE('',*,*,#2589,.F.);
#3212=ORIENTED_EDGE('',*,*,#2590,.T.);
#3213=ORIENTED_EDGE('',*,*,#2591,.F.);
#3214=ORIENTED_EDGE('',*,*,#2590,.F.);
#3215=ORIENTED_EDGE('',*,*,#2592,.F.);
#3216=ORIENTED_EDGE('',*,*,#2593,.T.);
#3217=ORIENTED_EDGE('',*,*,#2594,.F.);
#3218=ORIENTED_EDGE('',*,*,#2595,.F.);
#3219=ORIENTED_EDGE('',*,*,#2593,.F.);
#3220=ORIENTED_EDGE('',*,*,#2596,.F.);
#3221=ORIENTED_EDGE('',*,*,#2597,.F.);
#3222=ORIENTED_EDGE('',*,*,#2598,.T.);
#3223=ORIENTED_EDGE('',*,*,#2599,.F.);
#3224=ORIENTED_EDGE('',*,*,#2598,.F.);
#3225=ORIENTED_EDGE('',*,*,#2600,.F.);
#3226=ORIENTED_EDGE('',*,*,#2601,.T.);
#3227=ORIENTED_EDGE('',*,*,#2602,.F.);
#3228=ORIENTED_EDGE('',*,*,#2603,.F.);
#3229=ORIENTED_EDGE('',*,*,#2601,.F.);
#3230=ORIENTED_EDGE('',*,*,#2604,.F.);
#3231=ORIENTED_EDGE('',*,*,#2605,.F.);
#3232=ORIENTED_EDGE('',*,*,#2606,.T.);
#3233=ORIENTED_EDGE('',*,*,#2607,.F.);
#3234=ORIENTED_EDGE('',*,*,#2606,.F.);
#3235=ORIENTED_EDGE('',*,*,#2608,.F.);
#3236=ORIENTED_EDGE('',*,*,#2609,.T.);
#3237=ORIENTED_EDGE('',*,*,#2610,.F.);
#3238=ORIENTED_EDGE('',*,*,#2611,.F.);
#3239=ORIENTED_EDGE('',*,*,#2609,.F.);
#3240=ORIENTED_EDGE('',*,*,#2612,.F.);
#3241=ORIENTED_EDGE('',*,*,#2613,.F.);
#3242=ORIENTED_EDGE('',*,*,#2614,.T.);
#3243=ORIENTED_EDGE('',*,*,#2615,.F.);
#3244=ORIENTED_EDGE('',*,*,#2614,.F.);
#3245=ORIENTED_EDGE('',*,*,#2616,.F.);
#3246=ORIENTED_EDGE('',*,*,#2617,.T.);
#3247=ORIENTED_EDGE('',*,*,#2576,.F.);
#3248=ORIENTED_EDGE('',*,*,#2617,.F.);
#3249=ORIENTED_EDGE('',*,*,#2588,.T.);
#3250=ORIENTED_EDGE('',*,*,#2589,.T.);
#3251=ORIENTED_EDGE('',*,*,#2586,.T.);
#3252=ORIENTED_EDGE('',*,*,#2587,.T.);
#3253=ORIENTED_EDGE('',*,*,#2612,.T.);
#3254=ORIENTED_EDGE('',*,*,#2613,.T.);
#3255=ORIENTED_EDGE('',*,*,#2610,.T.);
#3256=ORIENTED_EDGE('',*,*,#2611,.T.);
#3257=ORIENTED_EDGE('',*,*,#2618,.F.);
#3258=ORIENTED_EDGE('',*,*,#2616,.T.);
#3259=ORIENTED_EDGE('',*,*,#2619,.F.);
#3260=ORIENTED_EDGE('',*,*,#2620,.F.);
#3261=ORIENTED_EDGE('',*,*,#2621,.T.);
#3262=ORIENTED_EDGE('',*,*,#2619,.T.);
#3263=ORIENTED_EDGE('',*,*,#2621,.F.);
#3264=ORIENTED_EDGE('',*,*,#2622,.F.);
#3265=ORIENTED_EDGE('',*,*,#2623,.T.);
#3266=ORIENTED_EDGE('',*,*,#2577,.F.);
#3267=ORIENTED_EDGE('',*,*,#2623,.F.);
#3268=ORIENTED_EDGE('',*,*,#2596,.T.);
#3269=ORIENTED_EDGE('',*,*,#2597,.T.);
#3270=ORIENTED_EDGE('',*,*,#2594,.T.);
#3271=ORIENTED_EDGE('',*,*,#2595,.T.);
#3272=ORIENTED_EDGE('',*,*,#2604,.T.);
#3273=ORIENTED_EDGE('',*,*,#2605,.T.);
#3274=ORIENTED_EDGE('',*,*,#2602,.T.);
#3275=ORIENTED_EDGE('',*,*,#2603,.T.);
#3276=ORIENTED_EDGE('',*,*,#2624,.F.);
#3277=ORIENTED_EDGE('',*,*,#2622,.T.);
#3278=ORIENTED_EDGE('',*,*,#2625,.F.);
#3279=ORIENTED_EDGE('',*,*,#2626,.F.);
#3280=ORIENTED_EDGE('',*,*,#2627,.T.);
#3281=ORIENTED_EDGE('',*,*,#2625,.T.);
#3282=ORIENTED_EDGE('',*,*,#2627,.F.);
#3283=ORIENTED_EDGE('',*,*,#2628,.F.);
#3284=ORIENTED_EDGE('',*,*,#2629,.T.);
#3285=ORIENTED_EDGE('',*,*,#2630,.F.);
#3286=ORIENTED_EDGE('',*,*,#2629,.F.);
#3287=ORIENTED_EDGE('',*,*,#2618,.T.);
#3288=ORIENTED_EDGE('',*,*,#2624,.T.);
#3289=ORIENTED_EDGE('',*,*,#2631,.F.);
#3290=ORIENTED_EDGE('',*,*,#2580,.T.);
#3291=ORIENTED_EDGE('',*,*,#2574,.F.);
#3292=ORIENTED_EDGE('',*,*,#2582,.F.);
#3293=ORIENTED_EDGE('',*,*,#2630,.T.);
#3294=ORIENTED_EDGE('',*,*,#2615,.T.);
#3295=ORIENTED_EDGE('',*,*,#2607,.T.);
#3296=ORIENTED_EDGE('',*,*,#2599,.T.);
#3297=ORIENTED_EDGE('',*,*,#2591,.T.);
#3298=ORIENTED_EDGE('',*,*,#2632,.T.);
#3299=ORIENTED_EDGE('',*,*,#2583,.T.);
#3300=ORIENTED_EDGE('',*,*,#2572,.F.);
#3301=ORIENTED_EDGE('',*,*,#2579,.F.);
#3302=ORIENTED_EDGE('',*,*,#2628,.T.);
#3303=ORIENTED_EDGE('',*,*,#2608,.T.);
#3304=ORIENTED_EDGE('',*,*,#2600,.T.);
#3305=ORIENTED_EDGE('',*,*,#2592,.T.);
#3306=ORIENTED_EDGE('',*,*,#2584,.T.);
#3307=ORIENTED_EDGE('',*,*,#2632,.F.);
#3308=ORIENTED_EDGE('',*,*,#2578,.F.);
#3309=ORIENTED_EDGE('',*,*,#2631,.T.);
#3310=ORIENTED_EDGE('',*,*,#2581,.F.);
#3311=ORIENTED_EDGE('',*,*,#2620,.T.);
#3312=ORIENTED_EDGE('',*,*,#2626,.T.);
#3313=ORIENTED_EDGE('',*,*,#2633,.F.);
#3314=ORIENTED_EDGE('',*,*,#2634,.F.);
#3315=ORIENTED_EDGE('',*,*,#2635,.F.);
#3316=ORIENTED_EDGE('',*,*,#2636,.F.);
#3317=ORIENTED_EDGE('',*,*,#2637,.F.);
#3318=ORIENTED_EDGE('',*,*,#2638,.F.);
#3319=ORIENTED_EDGE('',*,*,#2639,.F.);
#3320=ORIENTED_EDGE('',*,*,#2640,.F.);
#3321=ORIENTED_EDGE('',*,*,#2641,.F.);
#3322=ORIENTED_EDGE('',*,*,#2642,.F.);
#3323=ORIENTED_EDGE('',*,*,#2643,.F.);
#3324=ORIENTED_EDGE('',*,*,#2644,.F.);
#3325=ORIENTED_EDGE('',*,*,#2645,.F.);
#3326=ORIENTED_EDGE('',*,*,#2646,.F.);
#3327=ORIENTED_EDGE('',*,*,#2647,.F.);
#3328=ORIENTED_EDGE('',*,*,#2648,.F.);
#3329=ORIENTED_EDGE('',*,*,#2634,.T.);
#3330=ORIENTED_EDGE('',*,*,#2649,.F.);
#3331=ORIENTED_EDGE('',*,*,#2642,.T.);
#3332=ORIENTED_EDGE('',*,*,#2650,.F.);
#3333=ORIENTED_EDGE('',*,*,#2638,.T.);
#3334=ORIENTED_EDGE('',*,*,#2651,.F.);
#3335=ORIENTED_EDGE('',*,*,#2646,.T.);
#3336=ORIENTED_EDGE('',*,*,#2652,.F.);
#3337=ORIENTED_EDGE('',*,*,#2653,.F.);
#3338=ORIENTED_EDGE('',*,*,#2637,.T.);
#3339=ORIENTED_EDGE('',*,*,#2654,.F.);
#3340=ORIENTED_EDGE('',*,*,#2647,.T.);
#3341=ORIENTED_EDGE('',*,*,#2651,.T.);
#3342=ORIENTED_EDGE('',*,*,#2639,.T.);
#3343=ORIENTED_EDGE('',*,*,#2650,.T.);
#3344=ORIENTED_EDGE('',*,*,#2641,.T.);
#3345=ORIENTED_EDGE('',*,*,#2655,.F.);
#3346=ORIENTED_EDGE('',*,*,#2633,.T.);
#3347=ORIENTED_EDGE('',*,*,#2656,.F.);
#3348=ORIENTED_EDGE('',*,*,#2643,.T.);
#3349=ORIENTED_EDGE('',*,*,#2649,.T.);
#3350=ORIENTED_EDGE('',*,*,#2635,.T.);
#3351=ORIENTED_EDGE('',*,*,#2652,.T.);
#3352=ORIENTED_EDGE('',*,*,#2645,.T.);
#3353=ORIENTED_EDGE('',*,*,#2657,.F.);
#3354=ORIENTED_EDGE('',*,*,#2658,.F.);
#3355=ORIENTED_EDGE('',*,*,#2659,.T.);
#3356=ORIENTED_EDGE('',*,*,#2653,.T.);
#3357=ORIENTED_EDGE('',*,*,#2659,.F.);
#3358=ORIENTED_EDGE('',*,*,#2636,.T.);
#3359=ORIENTED_EDGE('',*,*,#2657,.T.);
#3360=ORIENTED_EDGE('',*,*,#2648,.T.);
#3361=ORIENTED_EDGE('',*,*,#2654,.T.);
#3362=ORIENTED_EDGE('',*,*,#2640,.T.);
#3363=ORIENTED_EDGE('',*,*,#2655,.T.);
#3364=ORIENTED_EDGE('',*,*,#2644,.T.);
#3365=ORIENTED_EDGE('',*,*,#2656,.T.);
#3366=ORIENTED_EDGE('',*,*,#2658,.T.);
#3367=ORIENTED_EDGE('',*,*,#2660,.F.);
#3368=ORIENTED_EDGE('',*,*,#2661,.F.);
#3369=ORIENTED_EDGE('',*,*,#2662,.F.);
#3370=ORIENTED_EDGE('',*,*,#2663,.F.);
#3371=ORIENTED_EDGE('',*,*,#2664,.F.);
#3372=ORIENTED_EDGE('',*,*,#2665,.F.);
#3373=ORIENTED_EDGE('',*,*,#2666,.F.);
#3374=ORIENTED_EDGE('',*,*,#2667,.F.);
#3375=ORIENTED_EDGE('',*,*,#2668,.F.);
#3376=ORIENTED_EDGE('',*,*,#2669,.F.);
#3377=ORIENTED_EDGE('',*,*,#2670,.F.);
#3378=ORIENTED_EDGE('',*,*,#2671,.F.);
#3379=ORIENTED_EDGE('',*,*,#2672,.F.);
#3380=ORIENTED_EDGE('',*,*,#2673,.F.);
#3381=ORIENTED_EDGE('',*,*,#2674,.F.);
#3382=ORIENTED_EDGE('',*,*,#2675,.F.);
#3383=ORIENTED_EDGE('',*,*,#2661,.T.);
#3384=ORIENTED_EDGE('',*,*,#2676,.F.);
#3385=ORIENTED_EDGE('',*,*,#2669,.T.);
#3386=ORIENTED_EDGE('',*,*,#2677,.F.);
#3387=ORIENTED_EDGE('',*,*,#2665,.T.);
#3388=ORIENTED_EDGE('',*,*,#2678,.F.);
#3389=ORIENTED_EDGE('',*,*,#2673,.T.);
#3390=ORIENTED_EDGE('',*,*,#2679,.F.);
#3391=ORIENTED_EDGE('',*,*,#2680,.F.);
#3392=ORIENTED_EDGE('',*,*,#2664,.T.);
#3393=ORIENTED_EDGE('',*,*,#2681,.F.);
#3394=ORIENTED_EDGE('',*,*,#2674,.T.);
#3395=ORIENTED_EDGE('',*,*,#2678,.T.);
#3396=ORIENTED_EDGE('',*,*,#2666,.T.);
#3397=ORIENTED_EDGE('',*,*,#2677,.T.);
#3398=ORIENTED_EDGE('',*,*,#2668,.T.);
#3399=ORIENTED_EDGE('',*,*,#2682,.F.);
#3400=ORIENTED_EDGE('',*,*,#2660,.T.);
#3401=ORIENTED_EDGE('',*,*,#2683,.F.);
#3402=ORIENTED_EDGE('',*,*,#2670,.T.);
#3403=ORIENTED_EDGE('',*,*,#2676,.T.);
#3404=ORIENTED_EDGE('',*,*,#2662,.T.);
#3405=ORIENTED_EDGE('',*,*,#2679,.T.);
#3406=ORIENTED_EDGE('',*,*,#2672,.T.);
#3407=ORIENTED_EDGE('',*,*,#2684,.F.);
#3408=ORIENTED_EDGE('',*,*,#2685,.F.);
#3409=ORIENTED_EDGE('',*,*,#2686,.T.);
#3410=ORIENTED_EDGE('',*,*,#2680,.T.);
#3411=ORIENTED_EDGE('',*,*,#2686,.F.);
#3412=ORIENTED_EDGE('',*,*,#2663,.T.);
#3413=ORIENTED_EDGE('',*,*,#2684,.T.);
#3414=ORIENTED_EDGE('',*,*,#2675,.T.);
#3415=ORIENTED_EDGE('',*,*,#2681,.T.);
#3416=ORIENTED_EDGE('',*,*,#2667,.T.);
#3417=ORIENTED_EDGE('',*,*,#2682,.T.);
#3418=ORIENTED_EDGE('',*,*,#2671,.T.);
#3419=ORIENTED_EDGE('',*,*,#2683,.T.);
#3420=ORIENTED_EDGE('',*,*,#2685,.T.);
#3421=ORIENTED_EDGE('',*,*,#2687,.T.);
#3422=ORIENTED_EDGE('',*,*,#2688,.T.);
#3423=ORIENTED_EDGE('',*,*,#2689,.F.);
#3424=ORIENTED_EDGE('',*,*,#2688,.F.);
#3425=ORIENTED_EDGE('',*,*,#2689,.T.);
#3426=ORIENTED_EDGE('',*,*,#2687,.F.);
#3427=ORIENTED_EDGE('',*,*,#2690,.F.);
#3428=ORIENTED_EDGE('',*,*,#2691,.F.);
#3429=ORIENTED_EDGE('',*,*,#2692,.T.);
#3430=ORIENTED_EDGE('',*,*,#2693,.F.);
#3431=ORIENTED_EDGE('',*,*,#2694,.F.);
#3432=ORIENTED_EDGE('',*,*,#2692,.F.);
#3433=ORIENTED_EDGE('',*,*,#2695,.F.);
#3434=ORIENTED_EDGE('',*,*,#2696,.T.);
#3435=ORIENTED_EDGE('',*,*,#2697,.F.);
#3436=ORIENTED_EDGE('',*,*,#2696,.F.);
#3437=ORIENTED_EDGE('',*,*,#2695,.T.);
#3438=ORIENTED_EDGE('',*,*,#2698,.F.);
#3439=ORIENTED_EDGE('',*,*,#2699,.T.);
#3440=ORIENTED_EDGE('',*,*,#2700,.F.);
#3441=ORIENTED_EDGE('',*,*,#2699,.F.);
#3442=ORIENTED_EDGE('',*,*,#2698,.T.);
#3443=ORIENTED_EDGE('',*,*,#2701,.F.);
#3444=ORIENTED_EDGE('',*,*,#2702,.T.);
#3445=ORIENTED_EDGE('',*,*,#2703,.F.);
#3446=ORIENTED_EDGE('',*,*,#2702,.F.);
#3447=ORIENTED_EDGE('',*,*,#2701,.T.);
#3448=ORIENTED_EDGE('',*,*,#2704,.F.);
#3449=ORIENTED_EDGE('',*,*,#2705,.T.);
#3450=ORIENTED_EDGE('',*,*,#2706,.F.);
#3451=ORIENTED_EDGE('',*,*,#2705,.F.);
#3452=ORIENTED_EDGE('',*,*,#2704,.T.);
#3453=ORIENTED_EDGE('',*,*,#2707,.F.);
#3454=ORIENTED_EDGE('',*,*,#2708,.F.);
#3455=ORIENTED_EDGE('',*,*,#2709,.F.);
#3456=ORIENTED_EDGE('',*,*,#2710,.F.);
#3457=ORIENTED_EDGE('',*,*,#2711,.F.);
#3458=ORIENTED_EDGE('',*,*,#2708,.T.);
#3459=ORIENTED_EDGE('',*,*,#2712,.F.);
#3460=ORIENTED_EDGE('',*,*,#2713,.T.);
#3461=ORIENTED_EDGE('',*,*,#2714,.F.);
#3462=ORIENTED_EDGE('',*,*,#2715,.F.);
#3463=ORIENTED_EDGE('',*,*,#2716,.F.);
#3464=ORIENTED_EDGE('',*,*,#2713,.F.);
#3465=ORIENTED_EDGE('',*,*,#2717,.F.);
#3466=ORIENTED_EDGE('',*,*,#2718,.T.);
#3467=ORIENTED_EDGE('',*,*,#2719,.F.);
#3468=ORIENTED_EDGE('',*,*,#2720,.F.);
#3469=ORIENTED_EDGE('',*,*,#2721,.F.);
#3470=ORIENTED_EDGE('',*,*,#2718,.F.);
#3471=ORIENTED_EDGE('',*,*,#2722,.F.);
#3472=ORIENTED_EDGE('',*,*,#2723,.T.);
#3473=ORIENTED_EDGE('',*,*,#2724,.F.);
#3474=ORIENTED_EDGE('',*,*,#2725,.F.);
#3475=ORIENTED_EDGE('',*,*,#2726,.F.);
#3476=ORIENTED_EDGE('',*,*,#2723,.F.);
#3477=ORIENTED_EDGE('',*,*,#2727,.F.);
#3478=ORIENTED_EDGE('',*,*,#2728,.T.);
#3479=ORIENTED_EDGE('',*,*,#2729,.T.);
#3480=ORIENTED_EDGE('',*,*,#2709,.T.);
#3481=ORIENTED_EDGE('',*,*,#2707,.T.);
#3482=ORIENTED_EDGE('',*,*,#2711,.T.);
#3483=ORIENTED_EDGE('',*,*,#2730,.T.);
#3484=ORIENTED_EDGE('',*,*,#2724,.T.);
#3485=ORIENTED_EDGE('',*,*,#2726,.T.);
#3486=ORIENTED_EDGE('',*,*,#2722,.T.);
#3487=ORIENTED_EDGE('',*,*,#2731,.T.);
#3488=ORIENTED_EDGE('',*,*,#2719,.T.);
#3489=ORIENTED_EDGE('',*,*,#2721,.T.);
#3490=ORIENTED_EDGE('',*,*,#2717,.T.);
#3491=ORIENTED_EDGE('',*,*,#2732,.T.);
#3492=ORIENTED_EDGE('',*,*,#2714,.T.);
#3493=ORIENTED_EDGE('',*,*,#2716,.T.);
#3494=ORIENTED_EDGE('',*,*,#2712,.T.);
#3495=ORIENTED_EDGE('',*,*,#2733,.T.);
#3496=ORIENTED_EDGE('',*,*,#2728,.F.);
#3497=ORIENTED_EDGE('',*,*,#2734,.T.);
#3498=ORIENTED_EDGE('',*,*,#2733,.F.);
#3499=ORIENTED_EDGE('',*,*,#2715,.T.);
#3500=ORIENTED_EDGE('',*,*,#2732,.F.);
#3501=ORIENTED_EDGE('',*,*,#2720,.T.);
#3502=ORIENTED_EDGE('',*,*,#2731,.F.);
#3503=ORIENTED_EDGE('',*,*,#2725,.T.);
#3504=ORIENTED_EDGE('',*,*,#2730,.F.);
#3505=ORIENTED_EDGE('',*,*,#2710,.T.);
#3506=ORIENTED_EDGE('',*,*,#2729,.F.);
#3507=ORIENTED_EDGE('',*,*,#2735,.T.);
#3508=ORIENTED_EDGE('',*,*,#2736,.T.);
#3509=ORIENTED_EDGE('',*,*,#2737,.T.);
#3510=ORIENTED_EDGE('',*,*,#2738,.T.);
#3511=ORIENTED_EDGE('',*,*,#2739,.F.);
#3512=ORIENTED_EDGE('',*,*,#2740,.T.);
#3513=ORIENTED_EDGE('',*,*,#2735,.F.);
#3514=ORIENTED_EDGE('',*,*,#2740,.F.);
#3515=ORIENTED_EDGE('',*,*,#2741,.F.);
#3516=ORIENTED_EDGE('',*,*,#2742,.T.);
#3517=ORIENTED_EDGE('',*,*,#2738,.F.);
#3518=ORIENTED_EDGE('',*,*,#2742,.F.);
#3519=ORIENTED_EDGE('',*,*,#2743,.F.);
#3520=ORIENTED_EDGE('',*,*,#2744,.T.);
#3521=ORIENTED_EDGE('',*,*,#2736,.F.);
#3522=ORIENTED_EDGE('',*,*,#2744,.F.);
#3523=ORIENTED_EDGE('',*,*,#2745,.F.);
#3524=ORIENTED_EDGE('',*,*,#2746,.T.);
#3525=ORIENTED_EDGE('',*,*,#2737,.F.);
#3526=ORIENTED_EDGE('',*,*,#2746,.F.);
#3527=ORIENTED_EDGE('',*,*,#2747,.F.);
#3528=ORIENTED_EDGE('',*,*,#2748,.T.);
#3529=ORIENTED_EDGE('',*,*,#2749,.F.);
#3530=ORIENTED_EDGE('',*,*,#2748,.F.);
#3531=ORIENTED_EDGE('',*,*,#2747,.T.);
#3532=ORIENTED_EDGE('',*,*,#2750,.F.);
#3533=ORIENTED_EDGE('',*,*,#2734,.F.);
#3534=ORIENTED_EDGE('',*,*,#2751,.T.);
#3535=ORIENTED_EDGE('',*,*,#2752,.T.);
#3536=ORIENTED_EDGE('',*,*,#2751,.F.);
#3537=ORIENTED_EDGE('',*,*,#2693,.T.);
#3538=ORIENTED_EDGE('',*,*,#2694,.T.);
#3539=ORIENTED_EDGE('',*,*,#2750,.T.);
#3540=ORIENTED_EDGE('',*,*,#2753,.T.);
#3541=ORIENTED_EDGE('',*,*,#2754,.T.);
#3542=ORIENTED_EDGE('',*,*,#2753,.F.);
#3543=ORIENTED_EDGE('',*,*,#2690,.T.);
#3544=ORIENTED_EDGE('',*,*,#2691,.T.);
#3545=ORIENTED_EDGE('',*,*,#2727,.T.);
#3546=ORIENTED_EDGE('',*,*,#2749,.T.);
#3547=ORIENTED_EDGE('',*,*,#2706,.T.);
#3548=ORIENTED_EDGE('',*,*,#2703,.T.);
#3549=ORIENTED_EDGE('',*,*,#2700,.T.);
#3550=ORIENTED_EDGE('',*,*,#2697,.T.);
#3551=ORIENTED_EDGE('',*,*,#2752,.F.);
#3552=ORIENTED_EDGE('',*,*,#2754,.F.);
#3553=ORIENTED_EDGE('',*,*,#2745,.T.);
#3554=ORIENTED_EDGE('',*,*,#2743,.T.);
#3555=ORIENTED_EDGE('',*,*,#2741,.T.);
#3556=ORIENTED_EDGE('',*,*,#2739,.T.);
#3557=ORIENTED_EDGE('',*,*,#2755,.F.);
#3558=ORIENTED_EDGE('',*,*,#2756,.T.);
#3559=ORIENTED_EDGE('',*,*,#2757,.F.);
#3560=ORIENTED_EDGE('',*,*,#2756,.F.);
#3561=ORIENTED_EDGE('',*,*,#2755,.T.);
#3562=ORIENTED_EDGE('',*,*,#2758,.F.);
#3563=ORIENTED_EDGE('',*,*,#2759,.F.);
#3564=ORIENTED_EDGE('',*,*,#2760,.T.);
#3565=ORIENTED_EDGE('',*,*,#2761,.F.);
#3566=ORIENTED_EDGE('',*,*,#2760,.F.);
#3567=ORIENTED_EDGE('',*,*,#2759,.T.);
#3568=ORIENTED_EDGE('',*,*,#2762,.F.);
#3569=ORIENTED_EDGE('',*,*,#2763,.F.);
#3570=ORIENTED_EDGE('',*,*,#2764,.T.);
#3571=ORIENTED_EDGE('',*,*,#2765,.F.);
#3572=ORIENTED_EDGE('',*,*,#2764,.F.);
#3573=ORIENTED_EDGE('',*,*,#2763,.T.);
#3574=ORIENTED_EDGE('',*,*,#2766,.F.);
#3575=ORIENTED_EDGE('',*,*,#2767,.F.);
#3576=ORIENTED_EDGE('',*,*,#2768,.T.);
#3577=ORIENTED_EDGE('',*,*,#2769,.F.);
#3578=ORIENTED_EDGE('',*,*,#2768,.F.);
#3579=ORIENTED_EDGE('',*,*,#2767,.T.);
#3580=ORIENTED_EDGE('',*,*,#2770,.F.);
#3581=ORIENTED_EDGE('',*,*,#2771,.F.);
#3582=ORIENTED_EDGE('',*,*,#2772,.T.);
#3583=ORIENTED_EDGE('',*,*,#2758,.T.);
#3584=ORIENTED_EDGE('',*,*,#2772,.F.);
#3585=ORIENTED_EDGE('',*,*,#2773,.F.);
#3586=ORIENTED_EDGE('',*,*,#2774,.T.);
#3587=ORIENTED_EDGE('',*,*,#2762,.T.);
#3588=ORIENTED_EDGE('',*,*,#2774,.F.);
#3589=ORIENTED_EDGE('',*,*,#2775,.F.);
#3590=ORIENTED_EDGE('',*,*,#2776,.T.);
#3591=ORIENTED_EDGE('',*,*,#2766,.T.);
#3592=ORIENTED_EDGE('',*,*,#2776,.F.);
#3593=ORIENTED_EDGE('',*,*,#2777,.F.);
#3594=ORIENTED_EDGE('',*,*,#2778,.T.);
#3595=ORIENTED_EDGE('',*,*,#2770,.T.);
#3596=ORIENTED_EDGE('',*,*,#2778,.F.);
#3597=ORIENTED_EDGE('',*,*,#2779,.F.);
#3598=ORIENTED_EDGE('',*,*,#2780,.T.);
#3599=ORIENTED_EDGE('',*,*,#2781,.T.);
#3600=ORIENTED_EDGE('',*,*,#2780,.F.);
#3601=ORIENTED_EDGE('',*,*,#2781,.F.);
#3602=ORIENTED_EDGE('',*,*,#2782,.F.);
#3603=ORIENTED_EDGE('',*,*,#2783,.F.);
#3604=ORIENTED_EDGE('',*,*,#2784,.T.);
#3605=ORIENTED_EDGE('',*,*,#2782,.T.);
#3606=ORIENTED_EDGE('',*,*,#2784,.F.);
#3607=ORIENTED_EDGE('',*,*,#2785,.F.);
#3608=ORIENTED_EDGE('',*,*,#2786,.T.);
#3609=ORIENTED_EDGE('',*,*,#2787,.T.);
#3610=ORIENTED_EDGE('',*,*,#2786,.F.);
#3611=ORIENTED_EDGE('',*,*,#2785,.T.);
#3612=ORIENTED_EDGE('',*,*,#2783,.T.);
#3613=ORIENTED_EDGE('',*,*,#2769,.T.);
#3614=ORIENTED_EDGE('',*,*,#2765,.T.);
#3615=ORIENTED_EDGE('',*,*,#2761,.T.);
#3616=ORIENTED_EDGE('',*,*,#2757,.T.);
#3617=ORIENTED_EDGE('',*,*,#2787,.F.);
#3618=ORIENTED_EDGE('',*,*,#2779,.T.);
#3619=ORIENTED_EDGE('',*,*,#2777,.T.);
#3620=ORIENTED_EDGE('',*,*,#2775,.T.);
#3621=ORIENTED_EDGE('',*,*,#2773,.T.);
#3622=ORIENTED_EDGE('',*,*,#2771,.T.);
#3623=ORIENTED_EDGE('',*,*,#2788,.F.);
#3624=ORIENTED_EDGE('',*,*,#2789,.F.);
#3625=ORIENTED_EDGE('',*,*,#2790,.F.);
#3626=ORIENTED_EDGE('',*,*,#2791,.F.);
#3627=ORIENTED_EDGE('',*,*,#2792,.F.);
#3628=ORIENTED_EDGE('',*,*,#2791,.T.);
#3629=ORIENTED_EDGE('',*,*,#2793,.F.);
#3630=ORIENTED_EDGE('',*,*,#2794,.T.);
#3631=ORIENTED_EDGE('',*,*,#2795,.F.);
#3632=ORIENTED_EDGE('',*,*,#2794,.F.);
#3633=ORIENTED_EDGE('',*,*,#2796,.F.);
#3634=ORIENTED_EDGE('',*,*,#2797,.F.);
#3635=ORIENTED_EDGE('',*,*,#2798,.F.);
#3636=ORIENTED_EDGE('',*,*,#2797,.T.);
#3637=ORIENTED_EDGE('',*,*,#2799,.T.);
#3638=ORIENTED_EDGE('',*,*,#2789,.T.);
#3639=ORIENTED_EDGE('',*,*,#2799,.F.);
#3640=ORIENTED_EDGE('',*,*,#2796,.T.);
#3641=ORIENTED_EDGE('',*,*,#2793,.T.);
#3642=ORIENTED_EDGE('',*,*,#2790,.T.);
#3643=ORIENTED_EDGE('',*,*,#2800,.F.);
#3644=ORIENTED_EDGE('',*,*,#2801,.T.);
#3645=ORIENTED_EDGE('',*,*,#2802,.F.);
#3646=ORIENTED_EDGE('',*,*,#2803,.T.);
#3647=ORIENTED_EDGE('',*,*,#2800,.T.);
#3648=ORIENTED_EDGE('',*,*,#2803,.F.);
#3649=ORIENTED_EDGE('',*,*,#2802,.T.);
#3650=ORIENTED_EDGE('',*,*,#2804,.F.);
#3651=ORIENTED_EDGE('',*,*,#2805,.F.);
#3652=ORIENTED_EDGE('',*,*,#2806,.T.);
#3653=ORIENTED_EDGE('',*,*,#2804,.T.);
#3654=ORIENTED_EDGE('',*,*,#2806,.F.);
#3655=ORIENTED_EDGE('',*,*,#2807,.F.);
#3656=ORIENTED_EDGE('',*,*,#2805,.T.);
#3657=ORIENTED_EDGE('',*,*,#2808,.F.);
#3658=ORIENTED_EDGE('',*,*,#2809,.T.);
#3659=ORIENTED_EDGE('',*,*,#2807,.T.);
#3660=ORIENTED_EDGE('',*,*,#2809,.F.);
#3661=ORIENTED_EDGE('',*,*,#2808,.T.);
#3662=ORIENTED_EDGE('',*,*,#2810,.F.);
#3663=ORIENTED_EDGE('',*,*,#2811,.F.);
#3664=ORIENTED_EDGE('',*,*,#2812,.T.);
#3665=ORIENTED_EDGE('',*,*,#2810,.T.);
#3666=ORIENTED_EDGE('',*,*,#2812,.F.);
#3667=ORIENTED_EDGE('',*,*,#2813,.F.);
#3668=ORIENTED_EDGE('',*,*,#2811,.T.);
#3669=ORIENTED_EDGE('',*,*,#2814,.F.);
#3670=ORIENTED_EDGE('',*,*,#2815,.T.);
#3671=ORIENTED_EDGE('',*,*,#2813,.T.);
#3672=ORIENTED_EDGE('',*,*,#2815,.F.);
#3673=ORIENTED_EDGE('',*,*,#2814,.T.);
#3674=ORIENTED_EDGE('',*,*,#2816,.F.);
#3675=ORIENTED_EDGE('',*,*,#2816,.T.);
#3676=ORIENTED_EDGE('',*,*,#2817,.T.);
#3677=ORIENTED_EDGE('',*,*,#2801,.F.);
#3678=ORIENTED_EDGE('',*,*,#2817,.F.);
#3679=ORIENTED_EDGE('',*,*,#2795,.T.);
#3680=ORIENTED_EDGE('',*,*,#2798,.T.);
#3681=ORIENTED_EDGE('',*,*,#2788,.T.);
#3682=ORIENTED_EDGE('',*,*,#2792,.T.);
#3683=ORIENTED_EDGE('',*,*,#2818,.F.);
#3684=ORIENTED_EDGE('',*,*,#2819,.F.);
#3685=ORIENTED_EDGE('',*,*,#2820,.F.);
#3686=ORIENTED_EDGE('',*,*,#2821,.F.);
#3687=ORIENTED_EDGE('',*,*,#2822,.F.);
#3688=ORIENTED_EDGE('',*,*,#2821,.T.);
#3689=ORIENTED_EDGE('',*,*,#2823,.F.);
#3690=ORIENTED_EDGE('',*,*,#2824,.T.);
#3691=ORIENTED_EDGE('',*,*,#2825,.F.);
#3692=ORIENTED_EDGE('',*,*,#2824,.F.);
#3693=ORIENTED_EDGE('',*,*,#2826,.F.);
#3694=ORIENTED_EDGE('',*,*,#2827,.F.);
#3695=ORIENTED_EDGE('',*,*,#2828,.F.);
#3696=ORIENTED_EDGE('',*,*,#2827,.T.);
#3697=ORIENTED_EDGE('',*,*,#2829,.F.);
#3698=ORIENTED_EDGE('',*,*,#2819,.T.);
#3699=ORIENTED_EDGE('',*,*,#2830,.F.);
#3700=ORIENTED_EDGE('',*,*,#2831,.T.);
#3701=ORIENTED_EDGE('',*,*,#2832,.F.);
#3702=ORIENTED_EDGE('',*,*,#2833,.T.);
#3703=ORIENTED_EDGE('',*,*,#2830,.T.);
#3704=ORIENTED_EDGE('',*,*,#2833,.F.);
#3705=ORIENTED_EDGE('',*,*,#2825,.T.);
#3706=ORIENTED_EDGE('',*,*,#2828,.T.);
#3707=ORIENTED_EDGE('',*,*,#2818,.T.);
#3708=ORIENTED_EDGE('',*,*,#2822,.T.);
#3709=ORIENTED_EDGE('',*,*,#2832,.T.);
#3710=ORIENTED_EDGE('',*,*,#2834,.F.);
#3711=ORIENTED_EDGE('',*,*,#2834,.T.);
#3712=ORIENTED_EDGE('',*,*,#2835,.T.);
#3713=ORIENTED_EDGE('',*,*,#2831,.F.);
#3714=ORIENTED_EDGE('',*,*,#2835,.F.);
#3715=ORIENTED_EDGE('',*,*,#2826,.T.);
#3716=ORIENTED_EDGE('',*,*,#2823,.T.);
#3717=ORIENTED_EDGE('',*,*,#2820,.T.);
#3718=ORIENTED_EDGE('',*,*,#2829,.T.);
#3719=ORIENTED_EDGE('',*,*,#2836,.T.);
#3720=ORIENTED_EDGE('',*,*,#2837,.T.);
#3721=ORIENTED_EDGE('',*,*,#2838,.T.);
#3722=ORIENTED_EDGE('',*,*,#2839,.F.);
#3723=ORIENTED_EDGE('',*,*,#2840,.T.);
#3724=ORIENTED_EDGE('',*,*,#2841,.T.);
#3725=ORIENTED_EDGE('',*,*,#2842,.T.);
#3726=ORIENTED_EDGE('',*,*,#2837,.F.);
#3727=ORIENTED_EDGE('',*,*,#2843,.T.);
#3728=ORIENTED_EDGE('',*,*,#2844,.T.);
#3729=ORIENTED_EDGE('',*,*,#2845,.T.);
#3730=ORIENTED_EDGE('',*,*,#2841,.F.);
#3731=ORIENTED_EDGE('',*,*,#2846,.T.);
#3732=ORIENTED_EDGE('',*,*,#2847,.T.);
#3733=ORIENTED_EDGE('',*,*,#2848,.T.);
#3734=ORIENTED_EDGE('',*,*,#2844,.F.);
#3735=ORIENTED_EDGE('',*,*,#2849,.T.);
#3736=ORIENTED_EDGE('',*,*,#2850,.T.);
#3737=ORIENTED_EDGE('',*,*,#2851,.T.);
#3738=ORIENTED_EDGE('',*,*,#2847,.F.);
#3739=ORIENTED_EDGE('',*,*,#2852,.T.);
#3740=ORIENTED_EDGE('',*,*,#2839,.T.);
#3741=ORIENTED_EDGE('',*,*,#2853,.T.);
#3742=ORIENTED_EDGE('',*,*,#2850,.F.);
#3743=ORIENTED_EDGE('',*,*,#2852,.F.);
#3744=ORIENTED_EDGE('',*,*,#2849,.F.);
#3745=ORIENTED_EDGE('',*,*,#2846,.F.);
#3746=ORIENTED_EDGE('',*,*,#2843,.F.);
#3747=ORIENTED_EDGE('',*,*,#2840,.F.);
#3748=ORIENTED_EDGE('',*,*,#2836,.F.);
#3749=ORIENTED_EDGE('',*,*,#2853,.F.);
#3750=ORIENTED_EDGE('',*,*,#2838,.F.);
#3751=ORIENTED_EDGE('',*,*,#2842,.F.);
#3752=ORIENTED_EDGE('',*,*,#2845,.F.);
#3753=ORIENTED_EDGE('',*,*,#2848,.F.);
#3754=ORIENTED_EDGE('',*,*,#2851,.F.);
#3755=ORIENTED_EDGE('',*,*,#2854,.F.);
#3756=ORIENTED_EDGE('',*,*,#2855,.F.);
#3757=ORIENTED_EDGE('',*,*,#2856,.F.);
#3758=ORIENTED_EDGE('',*,*,#2857,.T.);
#3759=ORIENTED_EDGE('',*,*,#2855,.T.);
#3760=ORIENTED_EDGE('',*,*,#2857,.F.);
#3761=ORIENTED_EDGE('',*,*,#2858,.F.);
#3762=ORIENTED_EDGE('',*,*,#2859,.T.);
#3763=ORIENTED_EDGE('',*,*,#2856,.T.);
#3764=ORIENTED_EDGE('',*,*,#2859,.F.);
#3765=ORIENTED_EDGE('',*,*,#2860,.F.);
#3766=ORIENTED_EDGE('',*,*,#2861,.T.);
#3767=ORIENTED_EDGE('',*,*,#2858,.T.);
#3768=ORIENTED_EDGE('',*,*,#2861,.F.);
#3769=ORIENTED_EDGE('',*,*,#2860,.T.);
#3770=ORIENTED_EDGE('',*,*,#2862,.F.);
#3771=ORIENTED_EDGE('',*,*,#2863,.F.);
#3772=ORIENTED_EDGE('',*,*,#2864,.T.);
#3773=ORIENTED_EDGE('',*,*,#2862,.T.);
#3774=ORIENTED_EDGE('',*,*,#2864,.F.);
#3775=ORIENTED_EDGE('',*,*,#2854,.T.);
#3776=ORIENTED_EDGE('',*,*,#2865,.T.);
#3777=ORIENTED_EDGE('',*,*,#2863,.T.);
#3778=ORIENTED_EDGE('',*,*,#2865,.F.);
#3779=ORIENTED_EDGE('',*,*,#2866,.T.);
#3780=ORIENTED_EDGE('',*,*,#2867,.F.);
#3781=ORIENTED_EDGE('',*,*,#2868,.F.);
#3782=ORIENTED_EDGE('',*,*,#2869,.T.);
#3783=ORIENTED_EDGE('',*,*,#2866,.F.);
#3784=ORIENTED_EDGE('',*,*,#2870,.T.);
#3785=ORIENTED_EDGE('',*,*,#2868,.T.);
#3786=ORIENTED_EDGE('',*,*,#2870,.F.);
#3787=ORIENTED_EDGE('',*,*,#2871,.F.);
#3788=ORIENTED_EDGE('',*,*,#2872,.F.);
#3789=ORIENTED_EDGE('',*,*,#2869,.F.);
#3790=ORIENTED_EDGE('',*,*,#2873,.T.);
#3791=ORIENTED_EDGE('',*,*,#2871,.T.);
#3792=ORIENTED_EDGE('',*,*,#2873,.F.);
#3793=ORIENTED_EDGE('',*,*,#2872,.T.);
#3794=ORIENTED_EDGE('',*,*,#2874,.T.);
#3795=ORIENTED_EDGE('',*,*,#2875,.T.);
#3796=ORIENTED_EDGE('',*,*,#2874,.F.);
#3797=ORIENTED_EDGE('',*,*,#2876,.F.);
#3798=ORIENTED_EDGE('',*,*,#2877,.T.);
#3799=ORIENTED_EDGE('',*,*,#2867,.T.);
#3800=ORIENTED_EDGE('',*,*,#2877,.F.);
#3801=ORIENTED_EDGE('',*,*,#2876,.T.);
#3802=ORIENTED_EDGE('',*,*,#2875,.F.);
#3803=ORIENTED_EDGE('',*,*,#2878,.F.);
#3804=ORIENTED_EDGE('',*,*,#2879,.T.);
#3805=ORIENTED_EDGE('',*,*,#2880,.T.);
#3806=ORIENTED_EDGE('',*,*,#2879,.F.);
#3807=ORIENTED_EDGE('',*,*,#2881,.F.);
#3808=ORIENTED_EDGE('',*,*,#2882,.T.);
#3809=ORIENTED_EDGE('',*,*,#2883,.T.);
#3810=ORIENTED_EDGE('',*,*,#2882,.F.);
#3811=ORIENTED_EDGE('',*,*,#2881,.T.);
#3812=ORIENTED_EDGE('',*,*,#2878,.T.);
#3813=ORIENTED_EDGE('',*,*,#2883,.F.);
#3814=ORIENTED_EDGE('',*,*,#2880,.F.);
#3815=ORIENTED_EDGE('',*,*,#2884,.F.);
#3816=ORIENTED_EDGE('',*,*,#2885,.T.);
#3817=ORIENTED_EDGE('',*,*,#2886,.F.);
#3818=ORIENTED_EDGE('',*,*,#2887,.F.);
#3819=ORIENTED_EDGE('',*,*,#2888,.F.);
#3820=ORIENTED_EDGE('',*,*,#2889,.T.);
#3821=ORIENTED_EDGE('',*,*,#2890,.F.);
#3822=ORIENTED_EDGE('',*,*,#2891,.F.);
#3823=ORIENTED_EDGE('',*,*,#2889,.F.);
#3824=ORIENTED_EDGE('',*,*,#2892,.F.);
#3825=ORIENTED_EDGE('',*,*,#2885,.F.);
#3826=ORIENTED_EDGE('',*,*,#2893,.F.);
#3827=ORIENTED_EDGE('',*,*,#2887,.T.);
#3828=ORIENTED_EDGE('',*,*,#2894,.F.);
#3829=ORIENTED_EDGE('',*,*,#2895,.T.);
#3830=ORIENTED_EDGE('',*,*,#2896,.T.);
#3831=ORIENTED_EDGE('',*,*,#2895,.F.);
#3832=ORIENTED_EDGE('',*,*,#2892,.T.);
#3833=ORIENTED_EDGE('',*,*,#2888,.T.);
#3834=ORIENTED_EDGE('',*,*,#2893,.T.);
#3835=ORIENTED_EDGE('',*,*,#2886,.T.);
#3836=ORIENTED_EDGE('',*,*,#2884,.T.);
#3837=ORIENTED_EDGE('',*,*,#2897,.F.);
#3838=ORIENTED_EDGE('',*,*,#2898,.T.);
#3839=ORIENTED_EDGE('',*,*,#2899,.T.);
#3840=ORIENTED_EDGE('',*,*,#2898,.F.);
#3841=ORIENTED_EDGE('',*,*,#2890,.T.);
#3842=ORIENTED_EDGE('',*,*,#2891,.T.);
#3843=ORIENTED_EDGE('',*,*,#2897,.T.);
#3844=ORIENTED_EDGE('',*,*,#2894,.T.);
#3845=ORIENTED_EDGE('',*,*,#2899,.F.);
#3846=ORIENTED_EDGE('',*,*,#2896,.F.);
#3847=ORIENTED_EDGE('',*,*,#2900,.F.);
#3848=ORIENTED_EDGE('',*,*,#2901,.F.);
#3849=ORIENTED_EDGE('',*,*,#2902,.T.);
#3850=ORIENTED_EDGE('',*,*,#2903,.T.);
#3851=ORIENTED_EDGE('',*,*,#2904,.F.);
#3852=ORIENTED_EDGE('',*,*,#2905,.F.);
#3853=ORIENTED_EDGE('',*,*,#2906,.T.);
#3854=ORIENTED_EDGE('',*,*,#2907,.T.);
#3855=ORIENTED_EDGE('',*,*,#2902,.F.);
#3856=ORIENTED_EDGE('',*,*,#2908,.F.);
#3857=ORIENTED_EDGE('',*,*,#2909,.T.);
#3858=ORIENTED_EDGE('',*,*,#2910,.T.);
#3859=ORIENTED_EDGE('',*,*,#2906,.F.);
#3860=ORIENTED_EDGE('',*,*,#2911,.F.);
#3861=ORIENTED_EDGE('',*,*,#2912,.T.);
#3862=ORIENTED_EDGE('',*,*,#2913,.T.);
#3863=ORIENTED_EDGE('',*,*,#2909,.F.);
#3864=ORIENTED_EDGE('',*,*,#2914,.F.);
#3865=ORIENTED_EDGE('',*,*,#2915,.T.);
#3866=ORIENTED_EDGE('',*,*,#2916,.T.);
#3867=ORIENTED_EDGE('',*,*,#2912,.F.);
#3868=ORIENTED_EDGE('',*,*,#2917,.F.);
#3869=ORIENTED_EDGE('',*,*,#2904,.T.);
#3870=ORIENTED_EDGE('',*,*,#2918,.T.);
#3871=ORIENTED_EDGE('',*,*,#2915,.F.);
#3872=ORIENTED_EDGE('',*,*,#2918,.F.);
#3873=ORIENTED_EDGE('',*,*,#2903,.F.);
#3874=ORIENTED_EDGE('',*,*,#2907,.F.);
#3875=ORIENTED_EDGE('',*,*,#2910,.F.);
#3876=ORIENTED_EDGE('',*,*,#2913,.F.);
#3877=ORIENTED_EDGE('',*,*,#2916,.F.);
#3878=ORIENTED_EDGE('',*,*,#2919,.F.);
#3879=ORIENTED_EDGE('',*,*,#2901,.T.);
#3880=ORIENTED_EDGE('',*,*,#2917,.T.);
#3881=ORIENTED_EDGE('',*,*,#2914,.T.);
#3882=ORIENTED_EDGE('',*,*,#2911,.T.);
#3883=ORIENTED_EDGE('',*,*,#2908,.T.);
#3884=ORIENTED_EDGE('',*,*,#2905,.T.);
#3885=ORIENTED_EDGE('',*,*,#2920,.F.);
#3886=ORIENTED_EDGE('',*,*,#2921,.T.);
#3887=ORIENTED_EDGE('',*,*,#2919,.T.);
#3888=ORIENTED_EDGE('',*,*,#2921,.F.);
#3889=ORIENTED_EDGE('',*,*,#2900,.T.);
#3890=ORIENTED_EDGE('',*,*,#2922,.T.);
#3891=ORIENTED_EDGE('',*,*,#2920,.T.);
#3892=ORIENTED_EDGE('',*,*,#2922,.F.);
#3893=ORIENTED_EDGE('',*,*,#2923,.F.);
#3894=ORIENTED_EDGE('',*,*,#2924,.F.);
#3895=ORIENTED_EDGE('',*,*,#2925,.F.);
#3896=ORIENTED_EDGE('',*,*,#2926,.F.);
#3897=ORIENTED_EDGE('',*,*,#2927,.F.);
#3898=ORIENTED_EDGE('',*,*,#2928,.F.);
#3899=ORIENTED_EDGE('',*,*,#2929,.F.);
#3900=ORIENTED_EDGE('',*,*,#2924,.T.);
#3901=ORIENTED_EDGE('',*,*,#2930,.F.);
#3902=ORIENTED_EDGE('',*,*,#2926,.T.);
#3903=ORIENTED_EDGE('',*,*,#2931,.F.);
#3904=ORIENTED_EDGE('',*,*,#2932,.F.);
#3905=ORIENTED_EDGE('',*,*,#2933,.T.);
#3906=ORIENTED_EDGE('',*,*,#2934,.T.);
#3907=ORIENTED_EDGE('',*,*,#2935,.T.);
#3908=ORIENTED_EDGE('',*,*,#2928,.T.);
#3909=ORIENTED_EDGE('',*,*,#2936,.T.);
#3910=ORIENTED_EDGE('',*,*,#2937,.T.);
#3911=ORIENTED_EDGE('',*,*,#2938,.T.);
#3912=ORIENTED_EDGE('',*,*,#2932,.T.);
#3913=ORIENTED_EDGE('',*,*,#2939,.F.);
#3914=ORIENTED_EDGE('',*,*,#2927,.T.);
#3915=ORIENTED_EDGE('',*,*,#2923,.T.);
#3916=ORIENTED_EDGE('',*,*,#2929,.T.);
#3917=ORIENTED_EDGE('',*,*,#2935,.F.);
#3918=ORIENTED_EDGE('',*,*,#2940,.F.);
#3919=ORIENTED_EDGE('',*,*,#2941,.F.);
#3920=ORIENTED_EDGE('',*,*,#2942,.T.);
#3921=ORIENTED_EDGE('',*,*,#2943,.T.);
#3922=ORIENTED_EDGE('',*,*,#2944,.F.);
#3923=ORIENTED_EDGE('',*,*,#2945,.F.);
#3924=ORIENTED_EDGE('',*,*,#2946,.T.);
#3925=ORIENTED_EDGE('',*,*,#2936,.F.);
#3926=ORIENTED_EDGE('',*,*,#2947,.F.);
#3927=ORIENTED_EDGE('',*,*,#2948,.T.);
#3928=ORIENTED_EDGE('',*,*,#2949,.F.);
#3929=ORIENTED_EDGE('',*,*,#2948,.F.);
#3930=ORIENTED_EDGE('',*,*,#2950,.F.);
#3931=ORIENTED_EDGE('',*,*,#2951,.T.);
#3932=ORIENTED_EDGE('',*,*,#2952,.F.);
#3933=ORIENTED_EDGE('',*,*,#2951,.F.);
#3934=ORIENTED_EDGE('',*,*,#2953,.F.);
#3935=ORIENTED_EDGE('',*,*,#2954,.T.);
#3936=ORIENTED_EDGE('',*,*,#2941,.T.);
#3937=ORIENTED_EDGE('',*,*,#2955,.F.);
#3938=ORIENTED_EDGE('',*,*,#2940,.T.);
#3939=ORIENTED_EDGE('',*,*,#2934,.F.);
#3940=ORIENTED_EDGE('',*,*,#2956,.F.);
#3941=ORIENTED_EDGE('',*,*,#2955,.T.);
#3942=ORIENTED_EDGE('',*,*,#2952,.T.);
#3943=ORIENTED_EDGE('',*,*,#2957,.F.);
#3944=ORIENTED_EDGE('',*,*,#2958,.F.);
#3945=ORIENTED_EDGE('',*,*,#2942,.F.);
#3946=ORIENTED_EDGE('',*,*,#2954,.F.);
#3947=ORIENTED_EDGE('',*,*,#2950,.T.);
#3948=ORIENTED_EDGE('',*,*,#2930,.T.);
#3949=ORIENTED_EDGE('',*,*,#2938,.F.);
#3950=ORIENTED_EDGE('',*,*,#2959,.F.);
#3951=ORIENTED_EDGE('',*,*,#2960,.T.);
#3952=ORIENTED_EDGE('',*,*,#2961,.F.);
#3953=ORIENTED_EDGE('',*,*,#2962,.T.);
#3954=ORIENTED_EDGE('',*,*,#2957,.T.);
#3955=ORIENTED_EDGE('',*,*,#2953,.T.);
#3956=ORIENTED_EDGE('',*,*,#2956,.T.);
#3957=ORIENTED_EDGE('',*,*,#2933,.F.);
#3958=ORIENTED_EDGE('',*,*,#2931,.T.);
#3959=ORIENTED_EDGE('',*,*,#2925,.T.);
#3960=ORIENTED_EDGE('',*,*,#2945,.T.);
#3961=ORIENTED_EDGE('',*,*,#2963,.F.);
#3962=ORIENTED_EDGE('',*,*,#2960,.F.);
#3963=ORIENTED_EDGE('',*,*,#2964,.T.);
#3964=ORIENTED_EDGE('',*,*,#2959,.T.);
#3965=ORIENTED_EDGE('',*,*,#2937,.F.);
#3966=ORIENTED_EDGE('',*,*,#2946,.F.);
#3967=ORIENTED_EDGE('',*,*,#2964,.F.);
#3968=ORIENTED_EDGE('',*,*,#2947,.T.);
#3969=ORIENTED_EDGE('',*,*,#2944,.T.);
#3970=ORIENTED_EDGE('',*,*,#2965,.F.);
#3971=ORIENTED_EDGE('',*,*,#2961,.T.);
#3972=ORIENTED_EDGE('',*,*,#2963,.T.);
#3973=ORIENTED_EDGE('',*,*,#2949,.T.);
#3974=ORIENTED_EDGE('',*,*,#2966,.F.);
#3975=ORIENTED_EDGE('',*,*,#2967,.T.);
#3976=ORIENTED_EDGE('',*,*,#2939,.T.);
#3977=ORIENTED_EDGE('',*,*,#2967,.F.);
#3978=ORIENTED_EDGE('',*,*,#2966,.T.);
#3979=ORIENTED_EDGE('',*,*,#2958,.T.);
#3980=ORIENTED_EDGE('',*,*,#2962,.F.);
#3981=ORIENTED_EDGE('',*,*,#2965,.T.);
#3982=ORIENTED_EDGE('',*,*,#2943,.F.);
#3983=ORIENTED_EDGE('',*,*,#2968,.F.);
#3984=ORIENTED_EDGE('',*,*,#2969,.T.);
#3985=ORIENTED_EDGE('',*,*,#2970,.F.);
#3986=ORIENTED_EDGE('',*,*,#2969,.F.);
#3987=ORIENTED_EDGE('',*,*,#2968,.T.);
#3988=ORIENTED_EDGE('',*,*,#2971,.T.);
#3989=ORIENTED_EDGE('',*,*,#2972,.F.);
#3990=ORIENTED_EDGE('',*,*,#2971,.F.);
#3991=ORIENTED_EDGE('',*,*,#2973,.T.);
#3992=ORIENTED_EDGE('',*,*,#2974,.T.);
#3993=ORIENTED_EDGE('',*,*,#2973,.F.);
#3994=ORIENTED_EDGE('',*,*,#2974,.F.);
#3995=ORIENTED_EDGE('',*,*,#2975,.F.);
#3996=ORIENTED_EDGE('',*,*,#2976,.T.);
#3997=ORIENTED_EDGE('',*,*,#2972,.T.);
#3998=ORIENTED_EDGE('',*,*,#2976,.F.);
#3999=ORIENTED_EDGE('',*,*,#2975,.T.);
#4000=ORIENTED_EDGE('',*,*,#2970,.T.);
#4001=ORIENTED_EDGE('',*,*,#2977,.F.);
#4002=ORIENTED_EDGE('',*,*,#2978,.T.);
#4003=ORIENTED_EDGE('',*,*,#2979,.T.);
#4004=ORIENTED_EDGE('',*,*,#2978,.F.);
#4005=ORIENTED_EDGE('',*,*,#2980,.F.);
#4006=ORIENTED_EDGE('',*,*,#2981,.T.);
#4007=ORIENTED_EDGE('',*,*,#2982,.T.);
#4008=ORIENTED_EDGE('',*,*,#2981,.F.);
#4009=ORIENTED_EDGE('',*,*,#2980,.T.);
#4010=ORIENTED_EDGE('',*,*,#2977,.T.);
#4011=ORIENTED_EDGE('',*,*,#2982,.F.);
#4012=ORIENTED_EDGE('',*,*,#2979,.F.);
#4013=ORIENTED_EDGE('',*,*,#2983,.F.);
#4014=ORIENTED_EDGE('',*,*,#2984,.T.);
#4015=ORIENTED_EDGE('',*,*,#2985,.T.);
#4016=ORIENTED_EDGE('',*,*,#2984,.F.);
#4017=ORIENTED_EDGE('',*,*,#2986,.F.);
#4018=ORIENTED_EDGE('',*,*,#2987,.T.);
#4019=ORIENTED_EDGE('',*,*,#2988,.T.);
#4020=ORIENTED_EDGE('',*,*,#2987,.F.);
#4021=ORIENTED_EDGE('',*,*,#2986,.T.);
#4022=ORIENTED_EDGE('',*,*,#2983,.T.);
#4023=ORIENTED_EDGE('',*,*,#2988,.F.);
#4024=ORIENTED_EDGE('',*,*,#2985,.F.);
#4025=ORIENTED_EDGE('',*,*,#2989,.F.);
#4026=ORIENTED_EDGE('',*,*,#2990,.T.);
#4027=ORIENTED_EDGE('',*,*,#2991,.T.);
#4028=ORIENTED_EDGE('',*,*,#2990,.F.);
#4029=ORIENTED_EDGE('',*,*,#2992,.F.);
#4030=ORIENTED_EDGE('',*,*,#2993,.T.);
#4031=ORIENTED_EDGE('',*,*,#2994,.T.);
#4032=ORIENTED_EDGE('',*,*,#2993,.F.);
#4033=ORIENTED_EDGE('',*,*,#2992,.T.);
#4034=ORIENTED_EDGE('',*,*,#2989,.T.);
#4035=ORIENTED_EDGE('',*,*,#2994,.F.);
#4036=ORIENTED_EDGE('',*,*,#2991,.F.);
#4037=ORIENTED_EDGE('',*,*,#2995,.T.);
#4038=ORIENTED_EDGE('',*,*,#2996,.T.);
#4039=ORIENTED_EDGE('',*,*,#2997,.T.);
#4040=ORIENTED_EDGE('',*,*,#2998,.F.);
#4041=ORIENTED_EDGE('',*,*,#2999,.T.);
#4042=ORIENTED_EDGE('',*,*,#3000,.T.);
#4043=ORIENTED_EDGE('',*,*,#3001,.T.);
#4044=ORIENTED_EDGE('',*,*,#2996,.F.);
#4045=ORIENTED_EDGE('',*,*,#3002,.T.);
#4046=ORIENTED_EDGE('',*,*,#3003,.T.);
#4047=ORIENTED_EDGE('',*,*,#3004,.T.);
#4048=ORIENTED_EDGE('',*,*,#3000,.F.);
#4049=ORIENTED_EDGE('',*,*,#3005,.T.);
#4050=ORIENTED_EDGE('',*,*,#3006,.T.);
#4051=ORIENTED_EDGE('',*,*,#3007,.T.);
#4052=ORIENTED_EDGE('',*,*,#3003,.F.);
#4053=ORIENTED_EDGE('',*,*,#3008,.T.);
#4054=ORIENTED_EDGE('',*,*,#3009,.T.);
#4055=ORIENTED_EDGE('',*,*,#3010,.T.);
#4056=ORIENTED_EDGE('',*,*,#3006,.F.);
#4057=ORIENTED_EDGE('',*,*,#3011,.T.);
#4058=ORIENTED_EDGE('',*,*,#2998,.T.);
#4059=ORIENTED_EDGE('',*,*,#3012,.T.);
#4060=ORIENTED_EDGE('',*,*,#3009,.F.);
#4061=ORIENTED_EDGE('',*,*,#3011,.F.);
#4062=ORIENTED_EDGE('',*,*,#3008,.F.);
#4063=ORIENTED_EDGE('',*,*,#3005,.F.);
#4064=ORIENTED_EDGE('',*,*,#3002,.F.);
#4065=ORIENTED_EDGE('',*,*,#2999,.F.);
#4066=ORIENTED_EDGE('',*,*,#2995,.F.);
#4067=ORIENTED_EDGE('',*,*,#3012,.F.);
#4068=ORIENTED_EDGE('',*,*,#2997,.F.);
#4069=ORIENTED_EDGE('',*,*,#3001,.F.);
#4070=ORIENTED_EDGE('',*,*,#3004,.F.);
#4071=ORIENTED_EDGE('',*,*,#3007,.F.);
#4072=ORIENTED_EDGE('',*,*,#3010,.F.);
#4073=ORIENTED_EDGE('',*,*,#3013,.F.);
#4074=ORIENTED_EDGE('',*,*,#3014,.F.);
#4075=ORIENTED_EDGE('',*,*,#3015,.F.);
#4076=ORIENTED_EDGE('',*,*,#3016,.T.);
#4077=ORIENTED_EDGE('',*,*,#3014,.T.);
#4078=ORIENTED_EDGE('',*,*,#3016,.F.);
#4079=ORIENTED_EDGE('',*,*,#3017,.F.);
#4080=ORIENTED_EDGE('',*,*,#3018,.T.);
#4081=ORIENTED_EDGE('',*,*,#3015,.T.);
#4082=ORIENTED_EDGE('',*,*,#3018,.F.);
#4083=ORIENTED_EDGE('',*,*,#3019,.F.);
#4084=ORIENTED_EDGE('',*,*,#3020,.T.);
#4085=ORIENTED_EDGE('',*,*,#3017,.T.);
#4086=ORIENTED_EDGE('',*,*,#3020,.F.);
#4087=ORIENTED_EDGE('',*,*,#3019,.T.);
#4088=ORIENTED_EDGE('',*,*,#3021,.F.);
#4089=ORIENTED_EDGE('',*,*,#3022,.F.);
#4090=ORIENTED_EDGE('',*,*,#3023,.T.);
#4091=ORIENTED_EDGE('',*,*,#3021,.T.);
#4092=ORIENTED_EDGE('',*,*,#3023,.F.);
#4093=ORIENTED_EDGE('',*,*,#3013,.T.);
#4094=ORIENTED_EDGE('',*,*,#3024,.T.);
#4095=ORIENTED_EDGE('',*,*,#3022,.T.);
#4096=ORIENTED_EDGE('',*,*,#3024,.F.);
#4097=ORIENTED_EDGE('',*,*,#3025,.F.);
#4098=ORIENTED_EDGE('',*,*,#3026,.F.);
#4099=ORIENTED_EDGE('',*,*,#3027,.T.);
#4100=ORIENTED_EDGE('',*,*,#3028,.F.);
#4101=ORIENTED_EDGE('',*,*,#3029,.F.);
#4102=ORIENTED_EDGE('',*,*,#3027,.F.);
#4103=ORIENTED_EDGE('',*,*,#3028,.T.);
#4104=ORIENTED_EDGE('',*,*,#3029,.T.);
#4105=ORIENTED_EDGE('',*,*,#3030,.T.);
#4106=ORIENTED_EDGE('',*,*,#3031,.T.);
#4107=ORIENTED_EDGE('',*,*,#3030,.F.);
#4108=ORIENTED_EDGE('',*,*,#3032,.T.);
#4109=ORIENTED_EDGE('',*,*,#3033,.T.);
#4110=ORIENTED_EDGE('',*,*,#3034,.F.);
#4111=ORIENTED_EDGE('',*,*,#3033,.F.);
#4112=ORIENTED_EDGE('',*,*,#3034,.T.);
#4113=ORIENTED_EDGE('',*,*,#3035,.T.);
#4114=ORIENTED_EDGE('',*,*,#3036,.F.);
#4115=ORIENTED_EDGE('',*,*,#3035,.F.);
#4116=ORIENTED_EDGE('',*,*,#3031,.F.);
#4117=ORIENTED_EDGE('',*,*,#3036,.T.);
#4118=ORIENTED_EDGE('',*,*,#3037,.F.);
#4119=ORIENTED_EDGE('',*,*,#3038,.T.);
#4120=ORIENTED_EDGE('',*,*,#3025,.T.);
#4121=ORIENTED_EDGE('',*,*,#3026,.T.);
#4122=ORIENTED_EDGE('',*,*,#3038,.F.);
#4123=ORIENTED_EDGE('',*,*,#3037,.T.);
#4124=ORIENTED_EDGE('',*,*,#3039,.F.);
#4125=ORIENTED_EDGE('',*,*,#3039,.T.);
#4126=ORIENTED_EDGE('',*,*,#3040,.T.);
#4127=ORIENTED_EDGE('',*,*,#3032,.F.);
#4128=ORIENTED_EDGE('',*,*,#3040,.F.);
#4129=ORIENTED_EDGE('',*,*,#3041,.F.);
#4130=ORIENTED_EDGE('',*,*,#3042,.F.);
#4131=ORIENTED_EDGE('',*,*,#3043,.T.);
#4132=ORIENTED_EDGE('',*,*,#3044,.F.);
#4133=ORIENTED_EDGE('',*,*,#3045,.F.);
#4134=ORIENTED_EDGE('',*,*,#3043,.F.);
#4135=ORIENTED_EDGE('',*,*,#3046,.T.);
#4136=ORIENTED_EDGE('',*,*,#3047,.T.);
#4137=ORIENTED_EDGE('',*,*,#3044,.T.);
#4138=ORIENTED_EDGE('',*,*,#3045,.T.);
#4139=ORIENTED_EDGE('',*,*,#3047,.F.);
#4140=ORIENTED_EDGE('',*,*,#3048,.F.);
#4141=ORIENTED_EDGE('',*,*,#3049,.T.);
#4142=ORIENTED_EDGE('',*,*,#3050,.F.);
#4143=ORIENTED_EDGE('',*,*,#3051,.T.);
#4144=ORIENTED_EDGE('',*,*,#3048,.T.);
#4145=ORIENTED_EDGE('',*,*,#3051,.F.);
#4146=ORIENTED_EDGE('',*,*,#3052,.F.);
#4147=ORIENTED_EDGE('',*,*,#3053,.T.);
#4148=ORIENTED_EDGE('',*,*,#3050,.T.);
#4149=ORIENTED_EDGE('',*,*,#3053,.F.);
#4150=ORIENTED_EDGE('',*,*,#3054,.F.);
#4151=ORIENTED_EDGE('',*,*,#3055,.T.);
#4152=ORIENTED_EDGE('',*,*,#3052,.T.);
#4153=ORIENTED_EDGE('',*,*,#3055,.F.);
#4154=ORIENTED_EDGE('',*,*,#3054,.T.);
#4155=ORIENTED_EDGE('',*,*,#3046,.F.);
#4156=ORIENTED_EDGE('',*,*,#3041,.T.);
#4157=ORIENTED_EDGE('',*,*,#3042,.T.);
#4158=ORIENTED_EDGE('',*,*,#3056,.T.);
#4159=ORIENTED_EDGE('',*,*,#3049,.F.);
#4160=ORIENTED_EDGE('',*,*,#3056,.F.);
#4161=ORIENTED_EDGE('',*,*,#3057,.T.);
#4162=ORIENTED_EDGE('',*,*,#3057,.F.);
#4163=ORIENTED_EDGE('',*,*,#3058,.T.);
#4164=ORIENTED_EDGE('',*,*,#3058,.F.);
#4165=ORIENTED_EDGE('',*,*,#3059,.T.);
#4166=ORIENTED_EDGE('',*,*,#3059,.F.);
#4167=ORIENTED_EDGE('',*,*,#3060,.T.);
#4168=ORIENTED_EDGE('',*,*,#3060,.F.);
#4169=ORIENTED_EDGE('',*,*,#3061,.T.);
#4170=ORIENTED_EDGE('',*,*,#3061,.F.);
#4171=ORIENTED_EDGE('',*,*,#3062,.T.);
#4172=ORIENTED_EDGE('',*,*,#3062,.F.);
#4173=ORIENTED_EDGE('',*,*,#3063,.T.);
#4174=ORIENTED_EDGE('',*,*,#3063,.F.);
#4175=ORIENTED_EDGE('',*,*,#3064,.T.);
#4176=ORIENTED_EDGE('',*,*,#3064,.F.);
#4177=ORIENTED_EDGE('',*,*,#3065,.F.);
#4178=ORIENTED_EDGE('',*,*,#3066,.F.);
#4179=ORIENTED_EDGE('',*,*,#3067,.F.);
#4180=ORIENTED_EDGE('',*,*,#3068,.F.);
#4181=ORIENTED_EDGE('',*,*,#3067,.T.);
#4182=ORIENTED_EDGE('',*,*,#3069,.F.);
#4183=ORIENTED_EDGE('',*,*,#3070,.T.);
#4184=ORIENTED_EDGE('',*,*,#3071,.F.);
#4185=ORIENTED_EDGE('',*,*,#3072,.T.);
#4186=ORIENTED_EDGE('',*,*,#3073,.F.);
#4187=ORIENTED_EDGE('',*,*,#3074,.T.);
#4188=ORIENTED_EDGE('',*,*,#3075,.T.);
#4189=ORIENTED_EDGE('',*,*,#3076,.F.);
#4190=ORIENTED_EDGE('',*,*,#3075,.F.);
#4191=ORIENTED_EDGE('',*,*,#3077,.T.);
#4192=ORIENTED_EDGE('',*,*,#3078,.F.);
#4193=ORIENTED_EDGE('',*,*,#3079,.T.);
#4194=ORIENTED_EDGE('',*,*,#3080,.F.);
#4195=ORIENTED_EDGE('',*,*,#3081,.T.);
#4196=ORIENTED_EDGE('',*,*,#3082,.F.);
#4197=ORIENTED_EDGE('',*,*,#3083,.T.);
#4198=ORIENTED_EDGE('',*,*,#3084,.F.);
#4199=ORIENTED_EDGE('',*,*,#3085,.T.);
#4200=ORIENTED_EDGE('',*,*,#3086,.F.);
#4201=ORIENTED_EDGE('',*,*,#3066,.T.);
#4202=ORIENTED_EDGE('',*,*,#3087,.T.);
#4203=ORIENTED_EDGE('',*,*,#3088,.T.);
#4204=ORIENTED_EDGE('',*,*,#3069,.T.);
#4205=ORIENTED_EDGE('',*,*,#3089,.F.);
#4206=ORIENTED_EDGE('',*,*,#3090,.F.);
#4207=ORIENTED_EDGE('',*,*,#3070,.F.);
#4208=ORIENTED_EDGE('',*,*,#3088,.F.);
#4209=ORIENTED_EDGE('',*,*,#3090,.T.);
#4210=ORIENTED_EDGE('',*,*,#3091,.T.);
#4211=ORIENTED_EDGE('',*,*,#3092,.T.);
#4212=ORIENTED_EDGE('',*,*,#3071,.T.);
#4213=ORIENTED_EDGE('',*,*,#3093,.F.);
#4214=ORIENTED_EDGE('',*,*,#3094,.F.);
#4215=ORIENTED_EDGE('',*,*,#3072,.F.);
#4216=ORIENTED_EDGE('',*,*,#3092,.F.);
#4217=ORIENTED_EDGE('',*,*,#3094,.T.);
#4218=ORIENTED_EDGE('',*,*,#3095,.T.);
#4219=ORIENTED_EDGE('',*,*,#3096,.T.);
#4220=ORIENTED_EDGE('',*,*,#3073,.T.);
#4221=ORIENTED_EDGE('',*,*,#3097,.F.);
#4222=ORIENTED_EDGE('',*,*,#3098,.F.);
#4223=ORIENTED_EDGE('',*,*,#3077,.F.);
#4224=ORIENTED_EDGE('',*,*,#3074,.F.);
#4225=ORIENTED_EDGE('',*,*,#3096,.F.);
#4226=ORIENTED_EDGE('',*,*,#3099,.F.);
#4227=ORIENTED_EDGE('',*,*,#3098,.T.);
#4228=ORIENTED_EDGE('',*,*,#3100,.T.);
#4229=ORIENTED_EDGE('',*,*,#3101,.T.);
#4230=ORIENTED_EDGE('',*,*,#3078,.T.);
#4231=ORIENTED_EDGE('',*,*,#3102,.F.);
#4232=ORIENTED_EDGE('',*,*,#3103,.F.);
#4233=ORIENTED_EDGE('',*,*,#3079,.F.);
#4234=ORIENTED_EDGE('',*,*,#3101,.F.);
#4235=ORIENTED_EDGE('',*,*,#3103,.T.);
#4236=ORIENTED_EDGE('',*,*,#3104,.T.);
#4237=ORIENTED_EDGE('',*,*,#3105,.T.);
#4238=ORIENTED_EDGE('',*,*,#3080,.T.);
#4239=ORIENTED_EDGE('',*,*,#3106,.F.);
#4240=ORIENTED_EDGE('',*,*,#3107,.F.);
#4241=ORIENTED_EDGE('',*,*,#3081,.F.);
#4242=ORIENTED_EDGE('',*,*,#3105,.F.);
#4243=ORIENTED_EDGE('',*,*,#3107,.T.);
#4244=ORIENTED_EDGE('',*,*,#3108,.T.);
#4245=ORIENTED_EDGE('',*,*,#3109,.T.);
#4246=ORIENTED_EDGE('',*,*,#3082,.T.);
#4247=ORIENTED_EDGE('',*,*,#3083,.F.);
#4248=ORIENTED_EDGE('',*,*,#3109,.F.);
#4249=ORIENTED_EDGE('',*,*,#3110,.F.);
#4250=ORIENTED_EDGE('',*,*,#3111,.F.);
#4251=ORIENTED_EDGE('',*,*,#3112,.F.);
#4252=ORIENTED_EDGE('',*,*,#3113,.T.);
#4253=ORIENTED_EDGE('',*,*,#3099,.T.);
#4254=ORIENTED_EDGE('',*,*,#3095,.F.);
#4255=ORIENTED_EDGE('',*,*,#3093,.T.);
#4256=ORIENTED_EDGE('',*,*,#3091,.F.);
#4257=ORIENTED_EDGE('',*,*,#3089,.T.);
#4258=ORIENTED_EDGE('',*,*,#3087,.F.);
#4259=ORIENTED_EDGE('',*,*,#3065,.T.);
#4260=ORIENTED_EDGE('',*,*,#3114,.F.);
#4261=ORIENTED_EDGE('',*,*,#3115,.T.);
#4262=ORIENTED_EDGE('',*,*,#3116,.F.);
#4263=ORIENTED_EDGE('',*,*,#3110,.T.);
#4264=ORIENTED_EDGE('',*,*,#3108,.F.);
#4265=ORIENTED_EDGE('',*,*,#3106,.T.);
#4266=ORIENTED_EDGE('',*,*,#3104,.F.);
#4267=ORIENTED_EDGE('',*,*,#3102,.T.);
#4268=ORIENTED_EDGE('',*,*,#3100,.F.);
#4269=ORIENTED_EDGE('',*,*,#3097,.T.);
#4270=ORIENTED_EDGE('',*,*,#3113,.F.);
#4271=ORIENTED_EDGE('',*,*,#3068,.T.);
#4272=ORIENTED_EDGE('',*,*,#3086,.T.);
#4273=ORIENTED_EDGE('',*,*,#3117,.T.);
#4274=ORIENTED_EDGE('',*,*,#3114,.T.);
#4275=ORIENTED_EDGE('',*,*,#3085,.F.);
#4276=ORIENTED_EDGE('',*,*,#3118,.F.);
#4277=ORIENTED_EDGE('',*,*,#3115,.F.);
#4278=ORIENTED_EDGE('',*,*,#3117,.F.);
#4279=ORIENTED_EDGE('',*,*,#3076,.T.);
#4280=ORIENTED_EDGE('',*,*,#3112,.T.);
#4281=ORIENTED_EDGE('',*,*,#3111,.T.);
#4282=ORIENTED_EDGE('',*,*,#3116,.T.);
#4283=ORIENTED_EDGE('',*,*,#3118,.T.);
#4284=ORIENTED_EDGE('',*,*,#3084,.T.);
#4285=ORIENTED_EDGE('',*,*,#3119,.F.);
#4286=ORIENTED_EDGE('',*,*,#3120,.T.);
#4287=ORIENTED_EDGE('',*,*,#3121,.F.);
#4288=ORIENTED_EDGE('',*,*,#3122,.T.);
#4289=ORIENTED_EDGE('',*,*,#3119,.T.);
#4290=ORIENTED_EDGE('',*,*,#3122,.F.);
#4291=ORIENTED_EDGE('',*,*,#3121,.T.);
#4292=ORIENTED_EDGE('',*,*,#3123,.F.);
#4293=ORIENTED_EDGE('',*,*,#3123,.T.);
#4294=ORIENTED_EDGE('',*,*,#3124,.T.);
#4295=ORIENTED_EDGE('',*,*,#3120,.F.);
#4296=ORIENTED_EDGE('',*,*,#3124,.F.);
#4297=ORIENTED_EDGE('',*,*,#3125,.F.);
#4298=ORIENTED_EDGE('',*,*,#3126,.T.);
#4299=ORIENTED_EDGE('',*,*,#3127,.F.);
#4300=ORIENTED_EDGE('',*,*,#3128,.T.);
#4301=ORIENTED_EDGE('',*,*,#3125,.T.);
#4302=ORIENTED_EDGE('',*,*,#3128,.F.);
#4303=ORIENTED_EDGE('',*,*,#3127,.T.);
#4304=ORIENTED_EDGE('',*,*,#3129,.F.);
#4305=ORIENTED_EDGE('',*,*,#3129,.T.);
#4306=ORIENTED_EDGE('',*,*,#3130,.T.);
#4307=ORIENTED_EDGE('',*,*,#3126,.F.);
#4308=ORIENTED_EDGE('',*,*,#3130,.F.);
#4309=CYLINDRICAL_SURFACE('',#5019,0.210000000000001);
#4310=CYLINDRICAL_SURFACE('',#5022,0.210000000000001);
#4311=CYLINDRICAL_SURFACE('',#5025,0.21);
#4312=CYLINDRICAL_SURFACE('',#5028,0.21);
#4313=CYLINDRICAL_SURFACE('',#5031,0.21);
#4314=CYLINDRICAL_SURFACE('',#5034,0.21);
#4315=CYLINDRICAL_SURFACE('',#5049,0.165);
#4316=CYLINDRICAL_SURFACE('',#5051,0.165);
#4317=CYLINDRICAL_SURFACE('',#5053,0.165);
#4318=CYLINDRICAL_SURFACE('',#5055,0.165);
#4319=CYLINDRICAL_SURFACE('',#5057,0.165);
#4320=CYLINDRICAL_SURFACE('',#5059,0.165);
#4321=CYLINDRICAL_SURFACE('',#5061,0.165);
#4322=CYLINDRICAL_SURFACE('',#5063,0.165);
#4323=CYLINDRICAL_SURFACE('',#5065,0.5);
#4324=CYLINDRICAL_SURFACE('',#5069,0.275);
#4325=CYLINDRICAL_SURFACE('',#5071,0.5);
#4326=CYLINDRICAL_SURFACE('',#5075,0.275);
#4327=CYLINDRICAL_SURFACE('',#5077,1.05);
#4328=CYLINDRICAL_SURFACE('',#5084,0.225);
#4329=CYLINDRICAL_SURFACE('',#5087,0.225);
#4330=CYLINDRICAL_SURFACE('',#5090,0.225);
#4331=CYLINDRICAL_SURFACE('',#5093,0.225);
#4332=CYLINDRICAL_SURFACE('',#5102,1.9);
#4333=CYLINDRICAL_SURFACE('',#5104,1.9);
#4334=CYLINDRICAL_SURFACE('',#5106,1.9);
#4335=CYLINDRICAL_SURFACE('',#5108,1.9);
#4336=CYLINDRICAL_SURFACE('',#5110,0.62);
#4337=CYLINDRICAL_SURFACE('',#5114,0.225);
#4338=CYLINDRICAL_SURFACE('',#5117,0.225);
#4339=CYLINDRICAL_SURFACE('',#5120,0.225);
#4340=CYLINDRICAL_SURFACE('',#5123,0.225);
#4341=CYLINDRICAL_SURFACE('',#5132,1.9);
#4342=CYLINDRICAL_SURFACE('',#5134,1.9);
#4343=CYLINDRICAL_SURFACE('',#5136,1.9);
#4344=CYLINDRICAL_SURFACE('',#5138,1.9);
#4345=CYLINDRICAL_SURFACE('',#5140,0.62);
#4346=CYLINDRICAL_SURFACE('',#5149,0.25);
#4347=CYLINDRICAL_SURFACE('',#5150,0.165);
#4348=CYLINDRICAL_SURFACE('',#5154,0.165);
#4349=CYLINDRICAL_SURFACE('',#5158,0.165);
#4350=CYLINDRICAL_SURFACE('',#5162,0.165);
#4351=CYLINDRICAL_SURFACE('',#5169,0.525);
#4352=CYLINDRICAL_SURFACE('',#5171,0.525);
#4353=CYLINDRICAL_SURFACE('',#5176,0.525);
#4354=CYLINDRICAL_SURFACE('',#5181,0.525);
#4355=CYLINDRICAL_SURFACE('',#5186,2.2);
#4356=CYLINDRICAL_SURFACE('',#5199,0.275);
#4357=CYLINDRICAL_SURFACE('',#5201,0.275);
#4358=CYLINDRICAL_SURFACE('',#5203,0.275);
#4359=CYLINDRICAL_SURFACE('',#5205,0.275);
#4360=CYLINDRICAL_SURFACE('',#5207,1.5);
#4361=CYLINDRICAL_SURFACE('',#5212,3.);
#4362=CYLINDRICAL_SURFACE('',#5214,1.02);
#4363=CYLINDRICAL_SURFACE('',#5219,0.375);
#4364=CYLINDRICAL_SURFACE('',#5224,0.375);
#4365=CYLINDRICAL_SURFACE('',#5229,0.375);
#4366=CYLINDRICAL_SURFACE('',#5234,0.375);
#4367=CYLINDRICAL_SURFACE('',#5239,0.225);
#4368=CYLINDRICAL_SURFACE('',#5241,0.225);
#4369=CYLINDRICAL_SURFACE('',#5243,0.225);
#4370=CYLINDRICAL_SURFACE('',#5245,0.225);
#4371=CYLINDRICAL_SURFACE('',#5247,1.49);
#4372=CYLINDRICAL_SURFACE('',#5252,0.71);
#4373=CYLINDRICAL_SURFACE('',#5254,2.2);
#4374=CYLINDRICAL_SURFACE('',#5271,1.05);
#4375=CYLINDRICAL_SURFACE('',#5275,1.);
#4376=CYLINDRICAL_SURFACE('',#5279,1.05);
#4377=CYLINDRICAL_SURFACE('',#5283,1.);
#4378=CYLINDRICAL_SURFACE('',#5287,1.05);
#4379=CYLINDRICAL_SURFACE('',#5291,0.9);
#4380=CYLINDRICAL_SURFACE('',#5304,0.895);
#4381=CYLINDRICAL_SURFACE('',#5308,0.605);
#4382=CYLINDRICAL_SURFACE('',#5326,0.425);
#4383=CYLINDRICAL_SURFACE('',#5334,0.24505);
#4384=CYLINDRICAL_SURFACE('',#5343,2.99742622740447);
#4385=CYLINDRICAL_SURFACE('',#5347,0.7);
#4386=CYLINDRICAL_SURFACE('',#5348,0.5);
#4387=CYLINDRICAL_SURFACE('',#5350,0.5);
#4388=CYLINDRICAL_SURFACE('',#5355,0.505);
#4389=CYLINDRICAL_SURFACE('',#5358,0.7);
#4390=CYLINDRICAL_SURFACE('',#5366,0.165);
#4391=CYLINDRICAL_SURFACE('',#5369,0.505);
#4392=CYLINDRICAL_SURFACE('',#5372,0.9);
#4393=CYLINDRICAL_SURFACE('',#5391,0.1954);
#4394=CYLINDRICAL_SURFACE('',#5402,1.);
#4395=CYLINDRICAL_SURFACE('',#5404,1.);
#4396=CYLINDRICAL_SURFACE('',#5409,0.51);
#4397=CYLINDRICAL_SURFACE('',#5412,0.51);
#4398=CYLINDRICAL_SURFACE('',#5415,0.6);
#4399=CYLINDRICAL_SURFACE('',#5421,0.6);
#4400=CYLINDRICAL_SURFACE('',#5426,0.6);
#4401=CYLINDRICAL_SURFACE('',#5431,0.165);
#4402=CYLINDRICAL_SURFACE('',#5438,0.7);
#4403=CYLINDRICAL_SURFACE('',#5441,0.5);
#4404=CYLINDRICAL_SURFACE('',#5445,0.505);
#4405=CYLINDRICAL_SURFACE('',#5448,0.7);
#4406=CYLINDRICAL_SURFACE('',#5454,0.505);
#4407=CYLINDRICAL_SURFACE('',#5457,0.7);
#4408=CYLINDRICAL_SURFACE('',#5463,0.225);
#4409=CYLINDRICAL_SURFACE('',#5466,0.7);
#4410=CYLINDRICAL_SURFACE('',#5486,0.35);
#4411=CYLINDRICAL_SURFACE('',#5494,0.1954);
#4412=CYLINDRICAL_SURFACE('',#5510,0.976185);
#4413=CYLINDRICAL_SURFACE('',#5512,0.5);
#4414=CYLINDRICAL_SURFACE('',#5518,0.976185);
#4415=CYLINDRICAL_SURFACE('',#5530,1.023815);
#4416=CYLINDRICAL_SURFACE('',#5537,1.5);
#4417=CYLINDRICAL_SURFACE('',#5542,1.023815);
#4418=CYLINDRICAL_SURFACE('',#5564,1.019052);
#4419=CYLINDRICAL_SURFACE('',#5604,0.980948);
#4420=CYLINDRICAL_SURFACE('',#5618,1.013815);
#4421=CYLINDRICAL_SURFACE('',#5622,0.991185);
#4422=CYLINDRICAL_SURFACE('',#5626,1.013815);
#4423=CYLINDRICAL_SURFACE('',#5630,0.991185);
#4424=ADVANCED_FACE('',(#659),#4309,.F.);
#4425=ADVANCED_FACE('',(#660),#4310,.F.);
#4426=ADVANCED_FACE('',(#661),#4311,.F.);
#4427=ADVANCED_FACE('',(#662),#4312,.F.);
#4428=ADVANCED_FACE('',(#663),#4313,.F.);
#4429=ADVANCED_FACE('',(#664),#4314,.F.);
#4430=ADVANCED_FACE('',(#665),#523,.T.);
#4431=ADVANCED_FACE('',(#666),#524,.T.);
#4432=ADVANCED_FACE('',(#667),#525,.T.);
#4433=ADVANCED_FACE('',(#668),#526,.T.);
#4434=ADVANCED_FACE('',(#669,#401,#402,#403,#404,#405,#406),#527,.T.);
#4435=ADVANCED_FACE('',(#670,#407,#408,#409,#410,#411,#412),#528,.F.);
#4436=ADVANCED_FACE('',(#671,#413,#414),#529,.T.);
#4437=ADVANCED_FACE('',(#672),#530,.T.);
#4438=ADVANCED_FACE('',(#673),#531,.T.);
#4439=ADVANCED_FACE('',(#674),#4315,.F.);
#4440=ADVANCED_FACE('',(#675),#4316,.F.);
#4441=ADVANCED_FACE('',(#676),#4317,.F.);
#4442=ADVANCED_FACE('',(#677),#4318,.F.);
#4443=ADVANCED_FACE('',(#678),#4319,.F.);
#4444=ADVANCED_FACE('',(#679),#4320,.F.);
#4445=ADVANCED_FACE('',(#680),#4321,.F.);
#4446=ADVANCED_FACE('',(#681),#4322,.F.);
#4447=ADVANCED_FACE('',(#682,#415,#416,#417,#418,#419),#4323,.F.);
#4448=ADVANCED_FACE('',(#683,#420),#532,.T.);
#4449=ADVANCED_FACE('',(#684),#4324,.F.);
#4450=ADVANCED_FACE('',(#685,#421,#422,#423,#424,#425),#4325,.F.);
#4451=ADVANCED_FACE('',(#686,#426),#533,.T.);
#4452=ADVANCED_FACE('',(#687),#4326,.F.);
#4453=ADVANCED_FACE('',(#688,#427,#428),#4327,.F.);
#4454=ADVANCED_FACE('',(#689,#429,#430,#431,#432,#433),#534,.T.);
#4455=ADVANCED_FACE('',(#690,#434,#435,#436,#437,#438),#535,.T.);
#4456=ADVANCED_FACE('',(#691,#439,#440),#536,.F.);
#4457=ADVANCED_FACE('',(#692),#4328,.F.);
#4458=ADVANCED_FACE('',(#693),#4329,.F.);
#4459=ADVANCED_FACE('',(#694),#4330,.F.);
#4460=ADVANCED_FACE('',(#695),#4331,.F.);
#4461=ADVANCED_FACE('',(#696,#441),#537,.F.);
#4462=ADVANCED_FACE('',(#697),#4332,.T.);
#4463=ADVANCED_FACE('',(#698),#4333,.T.);
#4464=ADVANCED_FACE('',(#699),#4334,.T.);
#4465=ADVANCED_FACE('',(#700),#4335,.T.);
#4466=ADVANCED_FACE('',(#701),#4336,.F.);
#4467=ADVANCED_FACE('',(#702,#442),#538,.T.);
#4468=ADVANCED_FACE('',(#703),#4337,.F.);
#4469=ADVANCED_FACE('',(#704),#4338,.F.);
#4470=ADVANCED_FACE('',(#705),#4339,.F.);
#4471=ADVANCED_FACE('',(#706),#4340,.F.);
#4472=ADVANCED_FACE('',(#707,#443),#539,.F.);
#4473=ADVANCED_FACE('',(#708),#4341,.T.);
#4474=ADVANCED_FACE('',(#709),#4342,.T.);
#4475=ADVANCED_FACE('',(#710),#4343,.T.);
#4476=ADVANCED_FACE('',(#711),#4344,.T.);
#4477=ADVANCED_FACE('',(#712),#4345,.F.);
#4478=ADVANCED_FACE('',(#713,#444),#540,.T.);
#4479=ADVANCED_FACE('',(#714),#240,.T.);
#4480=ADVANCED_FACE('',(#715),#541,.T.);
#4481=ADVANCED_FACE('',(#716),#542,.F.);
#4482=ADVANCED_FACE('',(#717),#4346,.F.);
#4483=ADVANCED_FACE('',(#718),#4347,.F.);
#4484=ADVANCED_FACE('',(#719),#543,.T.);
#4485=ADVANCED_FACE('',(#720),#4348,.F.);
#4486=ADVANCED_FACE('',(#721),#544,.T.);
#4487=ADVANCED_FACE('',(#722),#4349,.F.);
#4488=ADVANCED_FACE('',(#723),#545,.T.);
#4489=ADVANCED_FACE('',(#724),#4350,.F.);
#4490=ADVANCED_FACE('',(#725),#546,.T.);
#4491=ADVANCED_FACE('',(#726),#547,.F.);
#4492=ADVANCED_FACE('',(#727),#4351,.F.);
#4493=ADVANCED_FACE('',(#728),#4352,.F.);
#4494=ADVANCED_FACE('',(#729),#548,.F.);
#4495=ADVANCED_FACE('',(#730),#4353,.F.);
#4496=ADVANCED_FACE('',(#731),#549,.F.);
#4497=ADVANCED_FACE('',(#732),#4354,.F.);
#4498=ADVANCED_FACE('',(#733),#550,.F.);
#4499=ADVANCED_FACE('',(#734),#4355,.T.);
#4500=ADVANCED_FACE('',(#735,#445,#446,#447,#448,#449),#551,.T.);
#4501=ADVANCED_FACE('',(#736),#4356,.F.);
#4502=ADVANCED_FACE('',(#737),#4357,.F.);
#4503=ADVANCED_FACE('',(#738),#4358,.F.);
#4504=ADVANCED_FACE('',(#739),#4359,.F.);
#4505=ADVANCED_FACE('',(#740),#4360,.F.);
#4506=ADVANCED_FACE('',(#741,#450),#552,.T.);
#4507=ADVANCED_FACE('',(#742,#451),#4361,.T.);
#4508=ADVANCED_FACE('',(#743,#452),#4362,.F.);
#4509=ADVANCED_FACE('',(#744,#453,#454,#455,#456,#457),#553,.T.);
#4510=ADVANCED_FACE('',(#745,#458,#459,#460,#461,#462),#554,.F.);
#4511=ADVANCED_FACE('',(#746),#4363,.F.);
#4512=ADVANCED_FACE('',(#747,#463),#555,.T.);
#4513=ADVANCED_FACE('',(#748),#4364,.F.);
#4514=ADVANCED_FACE('',(#749,#464),#556,.T.);
#4515=ADVANCED_FACE('',(#750),#4365,.F.);
#4516=ADVANCED_FACE('',(#751,#465),#557,.T.);
#4517=ADVANCED_FACE('',(#752),#4366,.F.);
#4518=ADVANCED_FACE('',(#753,#466),#558,.T.);
#4519=ADVANCED_FACE('',(#754),#4367,.F.);
#4520=ADVANCED_FACE('',(#755),#4368,.F.);
#4521=ADVANCED_FACE('',(#756),#4369,.F.);
#4522=ADVANCED_FACE('',(#757),#4370,.F.);
#4523=ADVANCED_FACE('',(#758),#4371,.T.);
#4524=ADVANCED_FACE('',(#759,#467),#559,.F.);
#4525=ADVANCED_FACE('',(#760),#4372,.F.);
#4526=ADVANCED_FACE('',(#761),#4373,.T.);
#4527=ADVANCED_FACE('',(#762,#468,#469,#470,#471,#472),#560,.T.);
#4528=ADVANCED_FACE('',(#763,#473,#474,#475,#476,#477),#561,.F.);
#4529=ADVANCED_FACE('',(#764),#562,.F.);
#4530=ADVANCED_FACE('',(#765),#563,.F.);
#4531=ADVANCED_FACE('',(#766),#564,.F.);
#4532=ADVANCED_FACE('',(#767),#565,.F.);
#4533=ADVANCED_FACE('',(#768),#566,.F.);
#4534=ADVANCED_FACE('',(#769,#478),#567,.T.);
#4535=ADVANCED_FACE('',(#770),#4374,.T.);
#4536=ADVANCED_FACE('',(#771,#479),#568,.T.);
#4537=ADVANCED_FACE('',(#772),#4375,.T.);
#4538=ADVANCED_FACE('',(#773,#480),#569,.T.);
#4539=ADVANCED_FACE('',(#774),#4376,.T.);
#4540=ADVANCED_FACE('',(#775,#481),#570,.T.);
#4541=ADVANCED_FACE('',(#776),#4377,.T.);
#4542=ADVANCED_FACE('',(#777,#482),#571,.T.);
#4543=ADVANCED_FACE('',(#778),#4378,.T.);
#4544=ADVANCED_FACE('',(#779,#483),#572,.T.);
#4545=ADVANCED_FACE('',(#780,#484),#4379,.F.);
#4546=ADVANCED_FACE('',(#781),#573,.F.);
#4547=ADVANCED_FACE('',(#782),#574,.F.);
#4548=ADVANCED_FACE('',(#783),#575,.F.);
#4549=ADVANCED_FACE('',(#784),#576,.F.);
#4550=ADVANCED_FACE('',(#785,#485),#577,.T.);
#4551=ADVANCED_FACE('',(#786,#486),#4380,.T.);
#4552=ADVANCED_FACE('',(#787,#487),#578,.T.);
#4553=ADVANCED_FACE('',(#788,#488),#4381,.F.);
#4554=ADVANCED_FACE('',(#789),#579,.F.);
#4555=ADVANCED_FACE('',(#790),#580,.F.);
#4556=ADVANCED_FACE('',(#791),#581,.F.);
#4557=ADVANCED_FACE('',(#792),#582,.F.);
#4558=ADVANCED_FACE('',(#793),#583,.F.);
#4559=ADVANCED_FACE('',(#794),#584,.F.);
#4560=ADVANCED_FACE('',(#795),#585,.F.);
#4561=ADVANCED_FACE('',(#796),#586,.F.);
#4562=ADVANCED_FACE('',(#797),#587,.F.);
#4563=ADVANCED_FACE('',(#798),#588,.T.);
#4564=ADVANCED_FACE('',(#799),#29,.T.);
#4565=ADVANCED_FACE('',(#800),#4382,.T.);
#4566=ADVANCED_FACE('',(#801),#30,.T.);
#4567=ADVANCED_FACE('',(#802,#489),#589,.T.);
#4568=ADVANCED_FACE('',(#803),#31,.T.);
#4569=ADVANCED_FACE('',(#804),#4383,.T.);
#4570=ADVANCED_FACE('',(#805,#490),#590,.T.);
#4571=ADVANCED_FACE('',(#806,#491),#591,.F.);
#4572=ADVANCED_FACE('',(#807),#4384,.T.);
#4573=ADVANCED_FACE('',(#808,#492),#592,.F.);
#4574=ADVANCED_FACE('',(#809),#4385,.T.);
#4575=ADVANCED_FACE('',(#810),#4386,.T.);
#4576=ADVANCED_FACE('',(#811),#4387,.T.);
#4577=ADVANCED_FACE('',(#812),#593,.T.);
#4578=ADVANCED_FACE('',(#813),#594,.F.);
#4579=ADVANCED_FACE('',(#814),#4388,.F.);
#4580=ADVANCED_FACE('',(#815),#4389,.T.);
#4581=ADVANCED_FACE('',(#816,#493),#595,.T.);
#4582=ADVANCED_FACE('',(#817,#494),#596,.F.);
#4583=ADVANCED_FACE('',(#818),#597,.T.);
#4584=ADVANCED_FACE('',(#819),#4390,.F.);
#4585=ADVANCED_FACE('',(#820),#598,.T.);
#4586=ADVANCED_FACE('',(#821,#495),#4391,.F.);
#4587=ADVANCED_FACE('',(#822,#496),#4392,.T.);
#4588=ADVANCED_FACE('',(#823,#497),#599,.T.);
#4589=ADVANCED_FACE('',(#824,#498),#600,.F.);
#4590=ADVANCED_FACE('',(#825),#601,.F.);
#4591=ADVANCED_FACE('',(#826),#602,.F.);
#4592=ADVANCED_FACE('',(#827),#603,.F.);
#4593=ADVANCED_FACE('',(#828),#604,.F.);
#4594=ADVANCED_FACE('',(#829),#605,.F.);
#4595=ADVANCED_FACE('',(#830),#606,.F.);
#4596=ADVANCED_FACE('',(#831),#607,.F.);
#4597=ADVANCED_FACE('',(#832),#608,.F.);
#4598=ADVANCED_FACE('',(#833,#499),#609,.T.);
#4599=ADVANCED_FACE('',(#834),#32,.T.);
#4600=ADVANCED_FACE('',(#835),#4393,.T.);
#4601=ADVANCED_FACE('',(#836),#610,.F.);
#4602=ADVANCED_FACE('',(#837),#611,.F.);
#4603=ADVANCED_FACE('',(#838),#4394,.T.);
#4604=ADVANCED_FACE('',(#839),#4395,.T.);
#4605=ADVANCED_FACE('',(#840,#500),#612,.T.);
#4606=ADVANCED_FACE('',(#841),#613,.T.);
#4607=ADVANCED_FACE('',(#842),#4396,.F.);
#4608=ADVANCED_FACE('',(#843),#4397,.F.);
#4609=ADVANCED_FACE('',(#844),#4398,.T.);
#4610=ADVANCED_FACE('',(#845,#501),#614,.T.);
#4611=ADVANCED_FACE('',(#846,#502),#615,.F.);
#4612=ADVANCED_FACE('',(#847),#616,.T.);
#4613=ADVANCED_FACE('',(#848),#4399,.T.);
#4614=ADVANCED_FACE('',(#849,#503),#617,.T.);
#4615=ADVANCED_FACE('',(#850,#504),#618,.T.);
#4616=ADVANCED_FACE('',(#851),#4400,.T.);
#4617=ADVANCED_FACE('',(#852),#619,.T.);
#4618=ADVANCED_FACE('',(#853),#620,.F.);
#4619=ADVANCED_FACE('',(#854),#4401,.F.);
#4620=ADVANCED_FACE('',(#855),#621,.T.);
#4621=ADVANCED_FACE('',(#856,#505),#622,.T.);
#4622=ADVANCED_FACE('',(#857),#4402,.T.);
#4623=ADVANCED_FACE('',(#858),#623,.F.);
#4624=ADVANCED_FACE('',(#859),#4403,.T.);
#4625=ADVANCED_FACE('',(#860,#506),#624,.T.);
#4626=ADVANCED_FACE('',(#861),#4404,.F.);
#4627=ADVANCED_FACE('',(#862),#4405,.T.);
#4628=ADVANCED_FACE('',(#863,#507),#625,.T.);
#4629=ADVANCED_FACE('',(#864,#508),#626,.F.);
#4630=ADVANCED_FACE('',(#865),#4406,.F.);
#4631=ADVANCED_FACE('',(#866),#4407,.T.);
#4632=ADVANCED_FACE('',(#867,#509),#627,.T.);
#4633=ADVANCED_FACE('',(#868,#510),#628,.F.);
#4634=ADVANCED_FACE('',(#869),#4408,.F.);
#4635=ADVANCED_FACE('',(#870),#4409,.T.);
#4636=ADVANCED_FACE('',(#871,#511),#629,.T.);
#4637=ADVANCED_FACE('',(#872,#512),#630,.F.);
#4638=ADVANCED_FACE('',(#873),#631,.F.);
#4639=ADVANCED_FACE('',(#874),#632,.F.);
#4640=ADVANCED_FACE('',(#875),#633,.F.);
#4641=ADVANCED_FACE('',(#876),#634,.F.);
#4642=ADVANCED_FACE('',(#877),#635,.F.);
#4643=ADVANCED_FACE('',(#878),#636,.F.);
#4644=ADVANCED_FACE('',(#879),#637,.F.);
#4645=ADVANCED_FACE('',(#880),#638,.F.);
#4646=ADVANCED_FACE('',(#881),#639,.F.);
#4647=ADVANCED_FACE('',(#882),#640,.T.);
#4648=ADVANCED_FACE('',(#883),#33,.T.);
#4649=ADVANCED_FACE('',(#884),#4410,.T.);
#4650=ADVANCED_FACE('',(#885),#34,.T.);
#4651=ADVANCED_FACE('',(#886,#513),#641,.T.);
#4652=ADVANCED_FACE('',(#887),#35,.T.);
#4653=ADVANCED_FACE('',(#888),#4411,.T.);
#4654=ADVANCED_FACE('',(#889),#27,.F.);
#4655=ADVANCED_FACE('',(#890),#4412,.T.);
#4656=ADVANCED_FACE('',(#891),#4413,.F.);
#4657=ADVANCED_FACE('',(#892),#36,.F.);
#4658=ADVANCED_FACE('',(#893,#514),#642,.T.);
#4659=ADVANCED_FACE('',(#894),#4414,.T.);
#4660=ADVANCED_FACE('',(#895,#515),#643,.T.);
#4661=ADVANCED_FACE('',(#896),#37,.F.);
#4662=ADVANCED_FACE('',(#897),#28,.F.);
#4663=ADVANCED_FACE('',(#898),#4415,.F.);
#4664=ADVANCED_FACE('',(#899,#516),#644,.T.);
#4665=ADVANCED_FACE('',(#900),#38,.T.);
#4666=ADVANCED_FACE('',(#901),#4416,.T.);
#4667=ADVANCED_FACE('',(#902),#39,.T.);
#4668=ADVANCED_FACE('',(#903,#517),#645,.T.);
#4669=ADVANCED_FACE('',(#904),#4417,.F.);
#4670=ADVANCED_FACE('',(#905),#11,.T.);
#4671=ADVANCED_FACE('',(#906),#12,.T.);
#4672=ADVANCED_FACE('',(#907),#13,.T.);
#4673=ADVANCED_FACE('',(#908),#14,.T.);
#4674=ADVANCED_FACE('',(#909),#15,.T.);
#4675=ADVANCED_FACE('',(#910),#16,.T.);
#4676=ADVANCED_FACE('',(#911),#17,.T.);
#4677=ADVANCED_FACE('',(#912),#18,.T.);
#4678=ADVANCED_FACE('',(#913),#19,.F.);
#4679=ADVANCED_FACE('',(#914),#4418,.T.);
#4680=ADVANCED_FACE('',(#915),#646,.T.);
#4681=ADVANCED_FACE('',(#916),#20,.F.);
#4682=ADVANCED_FACE('',(#917),#647,.T.);
#4683=ADVANCED_FACE('',(#918),#21,.F.);
#4684=ADVANCED_FACE('',(#919),#648,.T.);
#4685=ADVANCED_FACE('',(#920),#22,.F.);
#4686=ADVANCED_FACE('',(#921),#649,.T.);
#4687=ADVANCED_FACE('',(#922),#23,.F.);
#4688=ADVANCED_FACE('',(#923),#650,.T.);
#4689=ADVANCED_FACE('',(#924),#24,.F.);
#4690=ADVANCED_FACE('',(#925),#651,.T.);
#4691=ADVANCED_FACE('',(#926),#25,.F.);
#4692=ADVANCED_FACE('',(#927),#4419,.F.);
#4693=ADVANCED_FACE('',(#928),#652,.T.);
#4694=ADVANCED_FACE('',(#929),#26,.F.);
#4695=ADVANCED_FACE('',(#930,#518),#653,.T.);
#4696=ADVANCED_FACE('',(#931),#654,.T.);
#4697=ADVANCED_FACE('',(#932,#519),#655,.T.);
#4698=ADVANCED_FACE('',(#933),#4420,.T.);
#4699=ADVANCED_FACE('',(#934,#520),#656,.T.);
#4700=ADVANCED_FACE('',(#935),#4421,.F.);
#4701=ADVANCED_FACE('',(#936,#521),#657,.T.);
#4702=ADVANCED_FACE('',(#937),#4422,.T.);
#4703=ADVANCED_FACE('',(#938,#522),#658,.T.);
#4704=ADVANCED_FACE('',(#939),#4423,.F.);
#4705=CLOSED_SHELL('',(#4424,#4425,#4426,#4427,#4428,#4429,#4430,#4431,
#4432,#4433,#4434,#4435));
#4706=CLOSED_SHELL('',(#4436,#4437,#4438,#4439,#4440,#4441,#4442,#4443,
#4444,#4445,#4446,#4447,#4448,#4449,#4450,#4451,#4452,#4453,#4454,#4455,
#4456));
#4707=CLOSED_SHELL('',(#4457,#4458,#4459,#4460,#4461,#4462,#4463,#4464,
#4465,#4466,#4467));
#4708=CLOSED_SHELL('',(#4468,#4469,#4470,#4471,#4472,#4473,#4474,#4475,
#4476,#4477,#4478));
#4709=CLOSED_SHELL('',(#4479,#4480,#4481));
#4710=CLOSED_SHELL('',(#4482,#4483,#4484,#4485,#4486,#4487,#4488,#4489,
#4490,#4491,#4492,#4493,#4494,#4495,#4496,#4497,#4498,#4499,#4500,#4501,
#4502,#4503,#4504,#4505,#4506,#4507,#4508,#4509,#4510));
#4711=CLOSED_SHELL('',(#4511,#4512,#4513,#4514,#4515,#4516,#4517,#4518,
#4519,#4520,#4521,#4522,#4523,#4524,#4525,#4526,#4527,#4528));
#4712=CLOSED_SHELL('',(#4529,#4530,#4531,#4532,#4533,#4534,#4535,#4536,
#4537,#4538,#4539,#4540,#4541,#4542,#4543,#4544,#4545));
#4713=CLOSED_SHELL('',(#4546,#4547,#4548,#4549,#4550,#4551,#4552,#4553));
#4714=CLOSED_SHELL('',(#4554,#4555,#4556,#4557,#4558,#4559,#4560,#4561));
#4715=CLOSED_SHELL('',(#4562,#4563,#4564,#4565,#4566,#4567,#4568,#4569));
#4716=CLOSED_SHELL('',(#4570,#4571,#4572,#4573,#4574,#4575,#4576,#4577,
#4578));
#4717=CLOSED_SHELL('',(#4579,#4580,#4581,#4582));
#4718=CLOSED_SHELL('',(#4583,#4584,#4585,#4586,#4587,#4588,#4589));
#4719=CLOSED_SHELL('',(#4590,#4591,#4592,#4593,#4594,#4595,#4596,#4597,
#4598,#4599,#4600));
#4720=CLOSED_SHELL('',(#4601,#4602,#4603,#4604,#4605,#4606,#4607,#4608,
#4609,#4610,#4611,#4612,#4613,#4614,#4615,#4616,#4617,#4618));
#4721=CLOSED_SHELL('',(#4619,#4620,#4621,#4622,#4623,#4624,#4625));
#4722=CLOSED_SHELL('',(#4626,#4627,#4628,#4629));
#4723=CLOSED_SHELL('',(#4630,#4631,#4632,#4633));
#4724=CLOSED_SHELL('',(#4634,#4635,#4636,#4637));
#4725=CLOSED_SHELL('',(#4638,#4639,#4640,#4641,#4642,#4643,#4644,#4645));
#4726=CLOSED_SHELL('',(#4646,#4647,#4648,#4649,#4650,#4651,#4652,#4653));
#4727=CLOSED_SHELL('',(#4654,#4655,#4656,#4657,#4658,#4659,#4660,#4661));
#4728=CLOSED_SHELL('',(#4662,#4663,#4664,#4665,#4666,#4667,#4668,#4669));
#4729=CLOSED_SHELL('',(#4670));
#4730=CLOSED_SHELL('',(#4671));
#4731=CLOSED_SHELL('',(#4672));
#4732=CLOSED_SHELL('',(#4673));
#4733=CLOSED_SHELL('',(#4674));
#4734=CLOSED_SHELL('',(#4675));
#4735=CLOSED_SHELL('',(#4676));
#4736=CLOSED_SHELL('',(#4677));
#4737=CLOSED_SHELL('',(#4678,#4679,#4680,#4681,#4682,#4683,#4684,#4685,
#4686,#4687,#4688,#4689,#4690,#4691,#4692,#4693,#4694,#4695,#4696));
#4738=CLOSED_SHELL('',(#4697,#4698,#4699,#4700));
#4739=CLOSED_SHELL('',(#4701,#4702,#4703,#4704));
#4740=DERIVED_UNIT_ELEMENT(#4790,1.);
#4741=DERIVED_UNIT_ELEMENT(#11037,-3.);
#4742=DERIVED_UNIT_ELEMENT(#4790,1.);
#4743=DERIVED_UNIT_ELEMENT(#11037,-3.);
#4744=DERIVED_UNIT_ELEMENT(#4790,1.);
#4745=DERIVED_UNIT_ELEMENT(#11037,-3.);
#4746=DERIVED_UNIT_ELEMENT(#4790,1.);
#4747=DERIVED_UNIT_ELEMENT(#11037,-3.);
#4748=DERIVED_UNIT_ELEMENT(#4790,1.);
#4749=DERIVED_UNIT_ELEMENT(#11037,-3.);
#4750=DERIVED_UNIT_ELEMENT(#4790,1.);
#4751=DERIVED_UNIT_ELEMENT(#11037,-3.);
#4752=DERIVED_UNIT_ELEMENT(#4790,1.);
#4753=DERIVED_UNIT_ELEMENT(#11037,-3.);
#4754=DERIVED_UNIT_ELEMENT(#4790,1.);
#4755=DERIVED_UNIT_ELEMENT(#11037,-3.);
#4756=DERIVED_UNIT_ELEMENT(#4790,1.);
#4757=DERIVED_UNIT_ELEMENT(#11037,-3.);
#4758=DERIVED_UNIT_ELEMENT(#4790,1.);
#4759=DERIVED_UNIT_ELEMENT(#11037,-3.);
#4760=DERIVED_UNIT_ELEMENT(#4790,1.);
#4761=DERIVED_UNIT_ELEMENT(#11037,-3.);
#4762=DERIVED_UNIT_ELEMENT(#4790,1.);
#4763=DERIVED_UNIT_ELEMENT(#11037,-3.);
#4764=DERIVED_UNIT_ELEMENT(#4790,1.);
#4765=DERIVED_UNIT_ELEMENT(#11037,-3.);
#4766=DERIVED_UNIT_ELEMENT(#4790,1.);
#4767=DERIVED_UNIT_ELEMENT(#11037,-3.);
#4768=DERIVED_UNIT_ELEMENT(#4790,1.);
#4769=DERIVED_UNIT_ELEMENT(#11037,-3.);
#4770=DERIVED_UNIT_ELEMENT(#4790,1.);
#4771=DERIVED_UNIT_ELEMENT(#11037,-3.);
#4772=DERIVED_UNIT_ELEMENT(#4790,1.);
#4773=DERIVED_UNIT_ELEMENT(#11037,-3.);
#4774=DERIVED_UNIT_ELEMENT(#4790,1.);
#4775=DERIVED_UNIT_ELEMENT(#11037,-3.);
#4776=DERIVED_UNIT_ELEMENT(#4790,1.);
#4777=DERIVED_UNIT_ELEMENT(#11037,-3.);
#4778=DERIVED_UNIT_ELEMENT(#4790,1.);
#4779=DERIVED_UNIT_ELEMENT(#11037,-3.);
#4780=DERIVED_UNIT_ELEMENT(#4790,1.);
#4781=DERIVED_UNIT_ELEMENT(#11037,-3.);
#4782=DERIVED_UNIT_ELEMENT(#4790,1.);
#4783=DERIVED_UNIT_ELEMENT(#11037,-3.);
#4784=DERIVED_UNIT_ELEMENT(#4790,1.);
#4785=DERIVED_UNIT_ELEMENT(#11037,-3.);
#4786=DERIVED_UNIT_ELEMENT(#4790,1.);
#4787=DERIVED_UNIT_ELEMENT(#11037,-3.);
#4788=DERIVED_UNIT_ELEMENT(#4790,1.);
#4789=DERIVED_UNIT_ELEMENT(#11037,-3.);
#4790=(
MASS_UNIT()
NAMED_UNIT(*)
SI_UNIT(.KILO.,.GRAM.)
);
#4791=DERIVED_UNIT((#4740,#4741));
#4792=DERIVED_UNIT((#4742,#4743));
#4793=DERIVED_UNIT((#4744,#4745));
#4794=DERIVED_UNIT((#4746,#4747));
#4795=DERIVED_UNIT((#4748,#4749));
#4796=DERIVED_UNIT((#4750,#4751));
#4797=DERIVED_UNIT((#4752,#4753));
#4798=DERIVED_UNIT((#4754,#4755));
#4799=DERIVED_UNIT((#4756,#4757));
#4800=DERIVED_UNIT((#4758,#4759));
#4801=DERIVED_UNIT((#4760,#4761));
#4802=DERIVED_UNIT((#4762,#4763));
#4803=DERIVED_UNIT((#4764,#4765));
#4804=DERIVED_UNIT((#4766,#4767));
#4805=DERIVED_UNIT((#4768,#4769));
#4806=DERIVED_UNIT((#4770,#4771));
#4807=DERIVED_UNIT((#4772,#4773));
#4808=DERIVED_UNIT((#4774,#4775));
#4809=DERIVED_UNIT((#4776,#4777));
#4810=DERIVED_UNIT((#4778,#4779));
#4811=DERIVED_UNIT((#4780,#4781));
#4812=DERIVED_UNIT((#4782,#4783));
#4813=DERIVED_UNIT((#4784,#4785));
#4814=DERIVED_UNIT((#4786,#4787));
#4815=DERIVED_UNIT((#4788,#4789));
#4816=MEASURE_REPRESENTATION_ITEM('density measure',
POSITIVE_RATIO_MEASURE(7850.),#4791);
#4817=MEASURE_REPRESENTATION_ITEM('density measure',
POSITIVE_RATIO_MEASURE(7850.),#4792);
#4818=MEASURE_REPRESENTATION_ITEM('density measure',
POSITIVE_RATIO_MEASURE(7850.),#4793);
#4819=MEASURE_REPRESENTATION_ITEM('density measure',
POSITIVE_RATIO_MEASURE(7850.),#4794);
#4820=MEASURE_REPRESENTATION_ITEM('density measure',
POSITIVE_RATIO_MEASURE(7850.),#4795);
#4821=MEASURE_REPRESENTATION_ITEM('density measure',
POSITIVE_RATIO_MEASURE(7850.),#4796);
#4822=MEASURE_REPRESENTATION_ITEM('density measure',
POSITIVE_RATIO_MEASURE(7850.),#4797);
#4823=MEASURE_REPRESENTATION_ITEM('density measure',
POSITIVE_RATIO_MEASURE(7850.),#4798);
#4824=MEASURE_REPRESENTATION_ITEM('density measure',
POSITIVE_RATIO_MEASURE(7850.),#4799);
#4825=MEASURE_REPRESENTATION_ITEM('density measure',
POSITIVE_RATIO_MEASURE(7850.),#4800);
#4826=MEASURE_REPRESENTATION_ITEM('density measure',
POSITIVE_RATIO_MEASURE(7850.),#4801);
#4827=MEASURE_REPRESENTATION_ITEM('density measure',
POSITIVE_RATIO_MEASURE(7850.),#4802);
#4828=MEASURE_REPRESENTATION_ITEM('density measure',
POSITIVE_RATIO_MEASURE(7850.),#4803);
#4829=MEASURE_REPRESENTATION_ITEM('density measure',
POSITIVE_RATIO_MEASURE(7850.),#4804);
#4830=MEASURE_REPRESENTATION_ITEM('density measure',
POSITIVE_RATIO_MEASURE(7850.),#4805);
#4831=MEASURE_REPRESENTATION_ITEM('density measure',
POSITIVE_RATIO_MEASURE(7850.),#4806);
#4832=MEASURE_REPRESENTATION_ITEM('density measure',
POSITIVE_RATIO_MEASURE(7850.),#4807);
#4833=MEASURE_REPRESENTATION_ITEM('density measure',
POSITIVE_RATIO_MEASURE(7850.),#4808);
#4834=MEASURE_REPRESENTATION_ITEM('density measure',
POSITIVE_RATIO_MEASURE(7850.),#4809);
#4835=MEASURE_REPRESENTATION_ITEM('density measure',
POSITIVE_RATIO_MEASURE(7850.),#4810);
#4836=MEASURE_REPRESENTATION_ITEM('density measure',
POSITIVE_RATIO_MEASURE(7850.),#4811);
#4837=MEASURE_REPRESENTATION_ITEM('density measure',
POSITIVE_RATIO_MEASURE(7850.),#4812);
#4838=MEASURE_REPRESENTATION_ITEM('density measure',
POSITIVE_RATIO_MEASURE(7850.),#4813);
#4839=MEASURE_REPRESENTATION_ITEM('density measure',
POSITIVE_RATIO_MEASURE(7850.),#4814);
#4840=MEASURE_REPRESENTATION_ITEM('density measure',
POSITIVE_RATIO_MEASURE(7850.),#4815);
#4841=PROPERTY_DEFINITION_REPRESENTATION(#4966,#4891);
#4842=PROPERTY_DEFINITION_REPRESENTATION(#4967,#4892);
#4843=PROPERTY_DEFINITION_REPRESENTATION(#4968,#4893);
#4844=PROPERTY_DEFINITION_REPRESENTATION(#4969,#4894);
#4845=PROPERTY_DEFINITION_REPRESENTATION(#4970,#4895);
#4846=PROPERTY_DEFINITION_REPRESENTATION(#4971,#4896);
#4847=PROPERTY_DEFINITION_REPRESENTATION(#4972,#4897);
#4848=PROPERTY_DEFINITION_REPRESENTATION(#4973,#4898);
#4849=PROPERTY_DEFINITION_REPRESENTATION(#4974,#4899);
#4850=PROPERTY_DEFINITION_REPRESENTATION(#4975,#4900);
#4851=PROPERTY_DEFINITION_REPRESENTATION(#4976,#4901);
#4852=PROPERTY_DEFINITION_REPRESENTATION(#4977,#4902);
#4853=PROPERTY_DEFINITION_REPRESENTATION(#4978,#4903);
#4854=PROPERTY_DEFINITION_REPRESENTATION(#4979,#4904);
#4855=PROPERTY_DEFINITION_REPRESENTATION(#4980,#4905);
#4856=PROPERTY_DEFINITION_REPRESENTATION(#4981,#4906);
#4857=PROPERTY_DEFINITION_REPRESENTATION(#4982,#4907);
#4858=PROPERTY_DEFINITION_REPRESENTATION(#4983,#4908);
#4859=PROPERTY_DEFINITION_REPRESENTATION(#4984,#4909);
#4860=PROPERTY_DEFINITION_REPRESENTATION(#4985,#4910);
#4861=PROPERTY_DEFINITION_REPRESENTATION(#4986,#4911);
#4862=PROPERTY_DEFINITION_REPRESENTATION(#4987,#4912);
#4863=PROPERTY_DEFINITION_REPRESENTATION(#4988,#4913);
#4864=PROPERTY_DEFINITION_REPRESENTATION(#4989,#4914);
#4865=PROPERTY_DEFINITION_REPRESENTATION(#4990,#4915);
#4866=PROPERTY_DEFINITION_REPRESENTATION(#4991,#4916);
#4867=PROPERTY_DEFINITION_REPRESENTATION(#4992,#4917);
#4868=PROPERTY_DEFINITION_REPRESENTATION(#4993,#4918);
#4869=PROPERTY_DEFINITION_REPRESENTATION(#4994,#4919);
#4870=PROPERTY_DEFINITION_REPRESENTATION(#4995,#4920);
#4871=PROPERTY_DEFINITION_REPRESENTATION(#4996,#4921);
#4872=PROPERTY_DEFINITION_REPRESENTATION(#4997,#4922);
#4873=PROPERTY_DEFINITION_REPRESENTATION(#4998,#4923);
#4874=PROPERTY_DEFINITION_REPRESENTATION(#4999,#4924);
#4875=PROPERTY_DEFINITION_REPRESENTATION(#5000,#4925);
#4876=PROPERTY_DEFINITION_REPRESENTATION(#5001,#4926);
#4877=PROPERTY_DEFINITION_REPRESENTATION(#5002,#4927);
#4878=PROPERTY_DEFINITION_REPRESENTATION(#5003,#4928);
#4879=PROPERTY_DEFINITION_REPRESENTATION(#5004,#4929);
#4880=PROPERTY_DEFINITION_REPRESENTATION(#5005,#4930);
#4881=PROPERTY_DEFINITION_REPRESENTATION(#5006,#4931);
#4882=PROPERTY_DEFINITION_REPRESENTATION(#5007,#4932);
#4883=PROPERTY_DEFINITION_REPRESENTATION(#5008,#4933);
#4884=PROPERTY_DEFINITION_REPRESENTATION(#5009,#4934);
#4885=PROPERTY_DEFINITION_REPRESENTATION(#5010,#4935);
#4886=PROPERTY_DEFINITION_REPRESENTATION(#5011,#4936);
#4887=PROPERTY_DEFINITION_REPRESENTATION(#5012,#4937);
#4888=PROPERTY_DEFINITION_REPRESENTATION(#5013,#4938);
#4889=PROPERTY_DEFINITION_REPRESENTATION(#5014,#4939);
#4890=PROPERTY_DEFINITION_REPRESENTATION(#5015,#4940);
#4891=REPRESENTATION('material name',(#4941),#11005);
#4892=REPRESENTATION('density',(#4816),#11005);
#4893=REPRESENTATION('material name',(#4942),#11006);
#4894=REPRESENTATION('density',(#4817),#11006);
#4895=REPRESENTATION('material name',(#4943),#11007);
#4896=REPRESENTATION('density',(#4818),#11007);
#4897=REPRESENTATION('material name',(#4944),#11008);
#4898=REPRESENTATION('density',(#4819),#11008);
#4899=REPRESENTATION('material name',(#4945),#11009);
#4900=REPRESENTATION('density',(#4820),#11009);
#4901=REPRESENTATION('material name',(#4946),#11010);
#4902=REPRESENTATION('density',(#4821),#11010);
#4903=REPRESENTATION('material name',(#4947),#11011);
#4904=REPRESENTATION('density',(#4822),#11011);
#4905=REPRESENTATION('material name',(#4948),#11013);
#4906=REPRESENTATION('density',(#4823),#11013);
#4907=REPRESENTATION('material name',(#4949),#11014);
#4908=REPRESENTATION('density',(#4824),#11014);
#4909=REPRESENTATION('material name',(#4950),#11015);
#4910=REPRESENTATION('density',(#4825),#11015);
#4911=REPRESENTATION('material name',(#4951),#11017);
#4912=REPRESENTATION('density',(#4826),#11017);
#4913=REPRESENTATION('material name',(#4952),#11018);
#4914=REPRESENTATION('density',(#4827),#11018);
#4915=REPRESENTATION('material name',(#4953),#11019);
#4916=REPRESENTATION('density',(#4828),#11019);
#4917=REPRESENTATION('material name',(#4954),#11020);
#4918=REPRESENTATION('density',(#4829),#11020);
#4919=REPRESENTATION('material name',(#4955),#11022);
#4920=REPRESENTATION('density',(#4830),#11022);
#4921=REPRESENTATION('material name',(#4956),#11023);
#4922=REPRESENTATION('density',(#4831),#11023);
#4923=REPRESENTATION('material name',(#4957),#11024);
#4924=REPRESENTATION('density',(#4832),#11024);
#4925=REPRESENTATION('material name',(#4958),#11025);
#4926=REPRESENTATION('density',(#4833),#11025);
#4927=REPRESENTATION('material name',(#4959),#11026);
#4928=REPRESENTATION('density',(#4834),#11026);
#4929=REPRESENTATION('material name',(#4960),#11027);
#4930=REPRESENTATION('density',(#4835),#11027);
#4931=REPRESENTATION('material name',(#4961),#11030);
#4932=REPRESENTATION('density',(#4836),#11030);
#4933=REPRESENTATION('material name',(#4962),#11031);
#4934=REPRESENTATION('density',(#4837),#11031);
#4935=REPRESENTATION('material name',(#4963),#11032);
#4936=REPRESENTATION('density',(#4838),#11032);
#4937=REPRESENTATION('material name',(#4964),#11033);
#4938=REPRESENTATION('density',(#4839),#11033);
#4939=REPRESENTATION('material name',(#4965),#11034);
#4940=REPRESENTATION('density',(#4840),#11034);
#4941=DESCRIPTIVE_REPRESENTATION_ITEM('Steel','Steel');
#4942=DESCRIPTIVE_REPRESENTATION_ITEM('Steel','Steel');
#4943=DESCRIPTIVE_REPRESENTATION_ITEM('Steel','Steel');
#4944=DESCRIPTIVE_REPRESENTATION_ITEM('Steel','Steel');
#4945=DESCRIPTIVE_REPRESENTATION_ITEM('Steel','Steel');
#4946=DESCRIPTIVE_REPRESENTATION_ITEM('Steel','Steel');
#4947=DESCRIPTIVE_REPRESENTATION_ITEM('Steel','Steel');
#4948=DESCRIPTIVE_REPRESENTATION_ITEM('Steel','Steel');
#4949=DESCRIPTIVE_REPRESENTATION_ITEM('Steel','Steel');
#4950=DESCRIPTIVE_REPRESENTATION_ITEM('Steel','Steel');
#4951=DESCRIPTIVE_REPRESENTATION_ITEM('Steel','Steel');
#4952=DESCRIPTIVE_REPRESENTATION_ITEM('Steel','Steel');
#4953=DESCRIPTIVE_REPRESENTATION_ITEM('Steel','Steel');
#4954=DESCRIPTIVE_REPRESENTATION_ITEM('Steel','Steel');
#4955=DESCRIPTIVE_REPRESENTATION_ITEM('Steel','Steel');
#4956=DESCRIPTIVE_REPRESENTATION_ITEM('Steel','Steel');
#4957=DESCRIPTIVE_REPRESENTATION_ITEM('Steel','Steel');
#4958=DESCRIPTIVE_REPRESENTATION_ITEM('Steel','Steel');
#4959=DESCRIPTIVE_REPRESENTATION_ITEM('Steel','Steel');
#4960=DESCRIPTIVE_REPRESENTATION_ITEM('Steel','Steel');
#4961=DESCRIPTIVE_REPRESENTATION_ITEM('Steel','Steel');
#4962=DESCRIPTIVE_REPRESENTATION_ITEM('Steel','Steel');
#4963=DESCRIPTIVE_REPRESENTATION_ITEM('Steel','Steel');
#4964=DESCRIPTIVE_REPRESENTATION_ITEM('Steel','Steel');
#4965=DESCRIPTIVE_REPRESENTATION_ITEM('Steel','Steel');
#4966=PROPERTY_DEFINITION('material property','material name',#11188);
#4967=PROPERTY_DEFINITION('material property','density of part',#11188);
#4968=PROPERTY_DEFINITION('material property','material name',#11189);
#4969=PROPERTY_DEFINITION('material property','density of part',#11189);
#4970=PROPERTY_DEFINITION('material property','material name',#11190);
#4971=PROPERTY_DEFINITION('material property','density of part',#11190);
#4972=PROPERTY_DEFINITION('material property','material name',#11191);
#4973=PROPERTY_DEFINITION('material property','density of part',#11191);
#4974=PROPERTY_DEFINITION('material property','material name',#11192);
#4975=PROPERTY_DEFINITION('material property','density of part',#11192);
#4976=PROPERTY_DEFINITION('material property','material name',#11193);
#4977=PROPERTY_DEFINITION('material property','density of part',#11193);
#4978=PROPERTY_DEFINITION('material property','material name',#11194);
#4979=PROPERTY_DEFINITION('material property','density of part',#11194);
#4980=PROPERTY_DEFINITION('material property','material name',#11196);
#4981=PROPERTY_DEFINITION('material property','density of part',#11196);
#4982=PROPERTY_DEFINITION('material property','material name',#11197);
#4983=PROPERTY_DEFINITION('material property','density of part',#11197);
#4984=PROPERTY_DEFINITION('material property','material name',#11198);
#4985=PROPERTY_DEFINITION('material property','density of part',#11198);
#4986=PROPERTY_DEFINITION('material property','material name',#11200);
#4987=PROPERTY_DEFINITION('material property','density of part',#11200);
#4988=PROPERTY_DEFINITION('material property','material name',#11201);
#4989=PROPERTY_DEFINITION('material property','density of part',#11201);
#4990=PROPERTY_DEFINITION('material property','material name',#11202);
#4991=PROPERTY_DEFINITION('material property','density of part',#11202);
#4992=PROPERTY_DEFINITION('material property','material name',#11203);
#4993=PROPERTY_DEFINITION('material property','density of part',#11203);
#4994=PROPERTY_DEFINITION('material property','material name',#11205);
#4995=PROPERTY_DEFINITION('material property','density of part',#11205);
#4996=PROPERTY_DEFINITION('material property','material name',#11206);
#4997=PROPERTY_DEFINITION('material property','density of part',#11206);
#4998=PROPERTY_DEFINITION('material property','material name',#11207);
#4999=PROPERTY_DEFINITION('material property','density of part',#11207);
#5000=PROPERTY_DEFINITION('material property','material name',#11208);
#5001=PROPERTY_DEFINITION('material property','density of part',#11208);
#5002=PROPERTY_DEFINITION('material property','material name',#11209);
#5003=PROPERTY_DEFINITION('material property','density of part',#11209);
#5004=PROPERTY_DEFINITION('material property','material name',#11210);
#5005=PROPERTY_DEFINITION('material property','density of part',#11210);
#5006=PROPERTY_DEFINITION('material property','material name',#11213);
#5007=PROPERTY_DEFINITION('material property','density of part',#11213);
#5008=PROPERTY_DEFINITION('material property','material name',#11214);
#5009=PROPERTY_DEFINITION('material property','density of part',#11214);
#5010=PROPERTY_DEFINITION('material property','material name',#11215);
#5011=PROPERTY_DEFINITION('material property','density of part',#11215);
#5012=PROPERTY_DEFINITION('material property','material name',#11216);
#5013=PROPERTY_DEFINITION('material property','density of part',#11216);
#5014=PROPERTY_DEFINITION('material property','material name',#11217);
#5015=PROPERTY_DEFINITION('material property','density of part',#11217);
#5016=AXIS2_PLACEMENT_3D('',#7224,#5668,#5669);
#5017=AXIS2_PLACEMENT_3D('',#7225,#5670,#5671);
#5018=AXIS2_PLACEMENT_3D('',#7226,#5672,#5673);
#5019=AXIS2_PLACEMENT_3D('',#7227,#5674,#5675);
#5020=AXIS2_PLACEMENT_3D('',#7229,#5676,#5677);
#5021=AXIS2_PLACEMENT_3D('',#7232,#5679,#5680);
#5022=AXIS2_PLACEMENT_3D('',#7233,#5681,#5682);
#5023=AXIS2_PLACEMENT_3D('',#7235,#5683,#5684);
#5024=AXIS2_PLACEMENT_3D('',#7238,#5686,#5687);
#5025=AXIS2_PLACEMENT_3D('',#7239,#5688,#5689);
#5026=AXIS2_PLACEMENT_3D('',#7241,#5690,#5691);
#5027=AXIS2_PLACEMENT_3D('',#7244,#5693,#5694);
#5028=AXIS2_PLACEMENT_3D('',#7245,#5695,#5696);
#5029=AXIS2_PLACEMENT_3D('',#7247,#5697,#5698);
#5030=AXIS2_PLACEMENT_3D('',#7250,#5700,#5701);
#5031=AXIS2_PLACEMENT_3D('',#7251,#5702,#5703);
#5032=AXIS2_PLACEMENT_3D('',#7253,#5704,#5705);
#5033=AXIS2_PLACEMENT_3D('',#7256,#5707,#5708);
#5034=AXIS2_PLACEMENT_3D('',#7257,#5709,#5710);
#5035=AXIS2_PLACEMENT_3D('',#7259,#5711,#5712);
#5036=AXIS2_PLACEMENT_3D('',#7262,#5714,#5715);
#5037=AXIS2_PLACEMENT_3D('',#7263,#5716,#5717);
#5038=AXIS2_PLACEMENT_3D('',#7272,#5722,#5723);
#5039=AXIS2_PLACEMENT_3D('',#7278,#5727,#5728);
#5040=AXIS2_PLACEMENT_3D('',#7284,#5732,#5733);
#5041=AXIS2_PLACEMENT_3D('',#7287,#5736,#5737);
#5042=AXIS2_PLACEMENT_3D('',#7288,#5738,#5739);
#5043=AXIS2_PLACEMENT_3D('',#7289,#5740,#5741);
#5044=AXIS2_PLACEMENT_3D('',#7290,#5742,#5743);
#5045=AXIS2_PLACEMENT_3D('',#7300,#5748,#5749);
#5046=AXIS2_PLACEMENT_3D('',#7302,#5750,#5751);
#5047=AXIS2_PLACEMENT_3D('',#7303,#5752,#5753);
#5048=AXIS2_PLACEMENT_3D('',#7309,#5757,#5758);
#5049=AXIS2_PLACEMENT_3D('',#7315,#5762,#5763);
#5050=AXIS2_PLACEMENT_3D('',#7317,#5764,#5765);
#5051=AXIS2_PLACEMENT_3D('',#7361,#5767,#5768);
#5052=AXIS2_PLACEMENT_3D('',#7406,#5770,#5771);
#5053=AXIS2_PLACEMENT_3D('',#7407,#5772,#5773);
#5054=AXIS2_PLACEMENT_3D('',#7409,#5774,#5775);
#5055=AXIS2_PLACEMENT_3D('',#7453,#5777,#5778);
#5056=AXIS2_PLACEMENT_3D('',#7498,#5780,#5781);
#5057=AXIS2_PLACEMENT_3D('',#7499,#5782,#5783);
#5058=AXIS2_PLACEMENT_3D('',#7501,#5784,#5785);
#5059=AXIS2_PLACEMENT_3D('',#7545,#5787,#5788);
#5060=AXIS2_PLACEMENT_3D('',#7590,#5790,#5791);
#5061=AXIS2_PLACEMENT_3D('',#7591,#5792,#5793);
#5062=AXIS2_PLACEMENT_3D('',#7593,#5794,#5795);
#5063=AXIS2_PLACEMENT_3D('',#7637,#5797,#5798);
#5064=AXIS2_PLACEMENT_3D('',#7682,#5800,#5801);
#5065=AXIS2_PLACEMENT_3D('',#7683,#5802,#5803);
#5066=AXIS2_PLACEMENT_3D('',#7685,#5804,#5805);
#5067=AXIS2_PLACEMENT_3D('',#7730,#5807,#5808);
#5068=AXIS2_PLACEMENT_3D('',#7732,#5809,#5810);
#5069=AXIS2_PLACEMENT_3D('',#7733,#5811,#5812);
#5070=AXIS2_PLACEMENT_3D('',#7735,#5813,#5814);
#5071=AXIS2_PLACEMENT_3D('',#7737,#5816,#5817);
#5072=AXIS2_PLACEMENT_3D('',#7739,#5818,#5819);
#5073=AXIS2_PLACEMENT_3D('',#7784,#5821,#5822);
#5074=AXIS2_PLACEMENT_3D('',#7786,#5823,#5824);
#5075=AXIS2_PLACEMENT_3D('',#7787,#5825,#5826);
#5076=AXIS2_PLACEMENT_3D('',#7789,#5827,#5828);
#5077=AXIS2_PLACEMENT_3D('',#7791,#5830,#5831);
#5078=AXIS2_PLACEMENT_3D('',#7793,#5832,#5833);
#5079=AXIS2_PLACEMENT_3D('',#7796,#5835,#5836);
#5080=AXIS2_PLACEMENT_3D('',#7797,#5837,#5838);
#5081=AXIS2_PLACEMENT_3D('',#7799,#5840,#5841);
#5082=AXIS2_PLACEMENT_3D('',#7801,#5843,#5844);
#5083=AXIS2_PLACEMENT_3D('',#7802,#5845,#5846);
#5084=AXIS2_PLACEMENT_3D('',#7803,#5847,#5848);
#5085=AXIS2_PLACEMENT_3D('',#7808,#5850,#5851);
#5086=AXIS2_PLACEMENT_3D('',#7811,#5853,#5854);
#5087=AXIS2_PLACEMENT_3D('',#7812,#5855,#5856);
#5088=AXIS2_PLACEMENT_3D('',#7817,#5858,#5859);
#5089=AXIS2_PLACEMENT_3D('',#7820,#5861,#5862);
#5090=AXIS2_PLACEMENT_3D('',#7821,#5863,#5864);
#5091=AXIS2_PLACEMENT_3D('',#7826,#5866,#5867);
#5092=AXIS2_PLACEMENT_3D('',#7829,#5869,#5870);
#5093=AXIS2_PLACEMENT_3D('',#7830,#5871,#5872);
#5094=AXIS2_PLACEMENT_3D('',#7835,#5874,#5875);
#5095=AXIS2_PLACEMENT_3D('',#7838,#5877,#5878);
#5096=AXIS2_PLACEMENT_3D('',#7839,#5879,#5880);
#5097=AXIS2_PLACEMENT_3D('',#7840,#5881,#5882);
#5098=AXIS2_PLACEMENT_3D('',#7841,#5883,#5884);
#5099=AXIS2_PLACEMENT_3D('',#7842,#5885,#5886);
#5100=AXIS2_PLACEMENT_3D('',#7843,#5887,#5888);
#5101=AXIS2_PLACEMENT_3D('',#7845,#5889,#5890);
#5102=AXIS2_PLACEMENT_3D('',#7846,#5891,#5892);
#5103=AXIS2_PLACEMENT_3D('',#7847,#5893,#5894);
#5104=AXIS2_PLACEMENT_3D('',#7848,#5895,#5896);
#5105=AXIS2_PLACEMENT_3D('',#7849,#5897,#5898);
#5106=AXIS2_PLACEMENT_3D('',#7850,#5899,#5900);
#5107=AXIS2_PLACEMENT_3D('',#7851,#5901,#5902);
#5108=AXIS2_PLACEMENT_3D('',#7852,#5903,#5904);
#5109=AXIS2_PLACEMENT_3D('',#7853,#5905,#5906);
#5110=AXIS2_PLACEMENT_3D('',#7854,#5907,#5908);
#5111=AXIS2_PLACEMENT_3D('',#7856,#5909,#5910);
#5112=AXIS2_PLACEMENT_3D('',#7858,#5912,#5913);
#5113=AXIS2_PLACEMENT_3D('',#7859,#5914,#5915);
#5114=AXIS2_PLACEMENT_3D('',#7860,#5916,#5917);
#5115=AXIS2_PLACEMENT_3D('',#7865,#5919,#5920);
#5116=AXIS2_PLACEMENT_3D('',#7868,#5922,#5923);
#5117=AXIS2_PLACEMENT_3D('',#7869,#5924,#5925);
#5118=AXIS2_PLACEMENT_3D('',#7874,#5927,#5928);
#5119=AXIS2_PLACEMENT_3D('',#7877,#5930,#5931);
#5120=AXIS2_PLACEMENT_3D('',#7878,#5932,#5933);
#5121=AXIS2_PLACEMENT_3D('',#7883,#5935,#5936);
#5122=AXIS2_PLACEMENT_3D('',#7886,#5938,#5939);
#5123=AXIS2_PLACEMENT_3D('',#7887,#5940,#5941);
#5124=AXIS2_PLACEMENT_3D('',#7892,#5943,#5944);
#5125=AXIS2_PLACEMENT_3D('',#7895,#5946,#5947);
#5126=AXIS2_PLACEMENT_3D('',#7896,#5948,#5949);
#5127=AXIS2_PLACEMENT_3D('',#7897,#5950,#5951);
#5128=AXIS2_PLACEMENT_3D('',#7898,#5952,#5953);
#5129=AXIS2_PLACEMENT_3D('',#7899,#5954,#5955);
#5130=AXIS2_PLACEMENT_3D('',#7900,#5956,#5957);
#5131=AXIS2_PLACEMENT_3D('',#7902,#5958,#5959);
#5132=AXIS2_PLACEMENT_3D('',#7903,#5960,#5961);
#5133=AXIS2_PLACEMENT_3D('',#7904,#5962,#5963);
#5134=AXIS2_PLACEMENT_3D('',#7905,#5964,#5965);
#5135=AXIS2_PLACEMENT_3D('',#7906,#5966,#5967);
#5136=AXIS2_PLACEMENT_3D('',#7907,#5968,#5969);
#5137=AXIS2_PLACEMENT_3D('',#7908,#5970,#5971);
#5138=AXIS2_PLACEMENT_3D('',#7909,#5972,#5973);
#5139=AXIS2_PLACEMENT_3D('',#7910,#5974,#5975);
#5140=AXIS2_PLACEMENT_3D('',#7911,#5976,#5977);
#5141=AXIS2_PLACEMENT_3D('',#7913,#5978,#5979);
#5142=AXIS2_PLACEMENT_3D('',#7915,#5981,#5982);
#5143=AXIS2_PLACEMENT_3D('',#7916,#5983,#5984);
#5144=AXIS2_PLACEMENT_3D('',#9318,#5985,#5986);
#5145=AXIS2_PLACEMENT_3D('',#9460,#5987,#5988);
#5146=AXIS2_PLACEMENT_3D('',#9461,#5989,#5990);
#5147=AXIS2_PLACEMENT_3D('',#9462,#5991,#5992);
#5148=AXIS2_PLACEMENT_3D('',#9463,#5993,#5994);
#5149=AXIS2_PLACEMENT_3D('',#9464,#5995,#5996);
#5150=AXIS2_PLACEMENT_3D('',#9542,#5998,#5999);
#5151=AXIS2_PLACEMENT_3D('',#9544,#6000,#6001);
#5152=AXIS2_PLACEMENT_3D('',#9547,#6003,#6004);
#5153=AXIS2_PLACEMENT_3D('',#9548,#6005,#6006);
#5154=AXIS2_PLACEMENT_3D('',#9549,#6007,#6008);
#5155=AXIS2_PLACEMENT_3D('',#9551,#6009,#6010);
#5156=AXIS2_PLACEMENT_3D('',#9554,#6012,#6013);
#5157=AXIS2_PLACEMENT_3D('',#9555,#6014,#6015);
#5158=AXIS2_PLACEMENT_3D('',#9556,#6016,#6017);
#5159=AXIS2_PLACEMENT_3D('',#9558,#6018,#6019);
#5160=AXIS2_PLACEMENT_3D('',#9561,#6021,#6022);
#5161=AXIS2_PLACEMENT_3D('',#9562,#6023,#6024);
#5162=AXIS2_PLACEMENT_3D('',#9563,#6025,#6026);
#5163=AXIS2_PLACEMENT_3D('',#9565,#6027,#6028);
#5164=AXIS2_PLACEMENT_3D('',#9568,#6030,#6031);
#5165=AXIS2_PLACEMENT_3D('',#9569,#6032,#6033);
#5166=AXIS2_PLACEMENT_3D('',#9570,#6034,#6035);
#5167=AXIS2_PLACEMENT_3D('',#9573,#6036,#6037);
#5168=AXIS2_PLACEMENT_3D('',#9574,#6038,#6039);
#5169=AXIS2_PLACEMENT_3D('',#9575,#6040,#6041);
#5170=AXIS2_PLACEMENT_3D('',#9579,#6043,#6044);
#5171=AXIS2_PLACEMENT_3D('',#9581,#6046,#6047);
#5172=AXIS2_PLACEMENT_3D('',#9586,#6049,#6050);
#5173=AXIS2_PLACEMENT_3D('',#9589,#6052,#6053);
#5174=AXIS2_PLACEMENT_3D('',#9590,#6054,#6055);
#5175=AXIS2_PLACEMENT_3D('',#9591,#6056,#6057);
#5176=AXIS2_PLACEMENT_3D('',#9592,#6058,#6059);
#5177=AXIS2_PLACEMENT_3D('',#9597,#6061,#6062);
#5178=AXIS2_PLACEMENT_3D('',#9600,#6064,#6065);
#5179=AXIS2_PLACEMENT_3D('',#9601,#6066,#6067);
#5180=AXIS2_PLACEMENT_3D('',#9602,#6068,#6069);
#5181=AXIS2_PLACEMENT_3D('',#9603,#6070,#6071);
#5182=AXIS2_PLACEMENT_3D('',#9608,#6073,#6074);
#5183=AXIS2_PLACEMENT_3D('',#9611,#6076,#6077);
#5184=AXIS2_PLACEMENT_3D('',#9612,#6078,#6079);
#5185=AXIS2_PLACEMENT_3D('',#9613,#6080,#6081);
#5186=AXIS2_PLACEMENT_3D('',#9614,#6082,#6083);
#5187=AXIS2_PLACEMENT_3D('',#9616,#6084,#6085);
#5188=AXIS2_PLACEMENT_3D('',#9619,#6087,#6088);
#5189=AXIS2_PLACEMENT_3D('',#9620,#6089,#6090);
#5190=AXIS2_PLACEMENT_3D('',#9621,#6091,#6092);
#5191=AXIS2_PLACEMENT_3D('',#9622,#6093,#6094);
#5192=AXIS2_PLACEMENT_3D('',#9623,#6095,#6096);
#5193=AXIS2_PLACEMENT_3D('',#9624,#6097,#6098);
#5194=AXIS2_PLACEMENT_3D('',#9626,#6099,#6100);
#5195=AXIS2_PLACEMENT_3D('',#9628,#6101,#6102);
#5196=AXIS2_PLACEMENT_3D('',#9630,#6103,#6104);
#5197=AXIS2_PLACEMENT_3D('',#9632,#6105,#6106);
#5198=AXIS2_PLACEMENT_3D('',#9634,#6107,#6108);
#5199=AXIS2_PLACEMENT_3D('',#9635,#6109,#6110);
#5200=AXIS2_PLACEMENT_3D('',#9637,#6111,#6112);
#5201=AXIS2_PLACEMENT_3D('',#9639,#6114,#6115);
#5202=AXIS2_PLACEMENT_3D('',#9641,#6116,#6117);
#5203=AXIS2_PLACEMENT_3D('',#9643,#6119,#6120);
#5204=AXIS2_PLACEMENT_3D('',#9645,#6121,#6122);
#5205=AXIS2_PLACEMENT_3D('',#9647,#6124,#6125);
#5206=AXIS2_PLACEMENT_3D('',#9649,#6126,#6127);
#5207=AXIS2_PLACEMENT_3D('',#9651,#6129,#6130);
#5208=AXIS2_PLACEMENT_3D('',#9653,#6131,#6132);
#5209=AXIS2_PLACEMENT_3D('',#9656,#6134,#6135);
#5210=AXIS2_PLACEMENT_3D('',#9657,#6136,#6137);
#5211=AXIS2_PLACEMENT_3D('',#9659,#6138,#6139);
#5212=AXIS2_PLACEMENT_3D('',#9660,#6140,#6141);
#5213=AXIS2_PLACEMENT_3D('',#9663,#6143,#6144);
#5214=AXIS2_PLACEMENT_3D('',#9664,#6145,#6146);
#5215=AXIS2_PLACEMENT_3D('',#9667,#6148,#6149);
#5216=AXIS2_PLACEMENT_3D('',#9668,#6150,#6151);
#5217=AXIS2_PLACEMENT_3D('',#9669,#6152,#6153);
#5218=AXIS2_PLACEMENT_3D('',#9670,#6154,#6155);
#5219=AXIS2_PLACEMENT_3D('',#9671,#6156,#6157);
#5220=AXIS2_PLACEMENT_3D('',#9673,#6158,#6159);
#5221=AXIS2_PLACEMENT_3D('',#9676,#6161,#6162);
#5222=AXIS2_PLACEMENT_3D('',#9677,#6163,#6164);
#5223=AXIS2_PLACEMENT_3D('',#9679,#6165,#6166);
#5224=AXIS2_PLACEMENT_3D('',#9680,#6167,#6168);
#5225=AXIS2_PLACEMENT_3D('',#9682,#6169,#6170);
#5226=AXIS2_PLACEMENT_3D('',#9685,#6172,#6173);
#5227=AXIS2_PLACEMENT_3D('',#9686,#6174,#6175);
#5228=AXIS2_PLACEMENT_3D('',#9688,#6176,#6177);
#5229=AXIS2_PLACEMENT_3D('',#9689,#6178,#6179);
#5230=AXIS2_PLACEMENT_3D('',#9691,#6180,#6181);
#5231=AXIS2_PLACEMENT_3D('',#9694,#6183,#6184);
#5232=AXIS2_PLACEMENT_3D('',#9695,#6185,#6186);
#5233=AXIS2_PLACEMENT_3D('',#9697,#6187,#6188);
#5234=AXIS2_PLACEMENT_3D('',#9698,#6189,#6190);
#5235=AXIS2_PLACEMENT_3D('',#9700,#6191,#6192);
#5236=AXIS2_PLACEMENT_3D('',#9703,#6194,#6195);
#5237=AXIS2_PLACEMENT_3D('',#9704,#6196,#6197);
#5238=AXIS2_PLACEMENT_3D('',#9706,#6198,#6199);
#5239=AXIS2_PLACEMENT_3D('',#9707,#6200,#6201);
#5240=AXIS2_PLACEMENT_3D('',#9709,#6202,#6203);
#5241=AXIS2_PLACEMENT_3D('',#9711,#6205,#6206);
#5242=AXIS2_PLACEMENT_3D('',#9713,#6207,#6208);
#5243=AXIS2_PLACEMENT_3D('',#9715,#6210,#6211);
#5244=AXIS2_PLACEMENT_3D('',#9717,#6212,#6213);
#5245=AXIS2_PLACEMENT_3D('',#9719,#6215,#6216);
#5246=AXIS2_PLACEMENT_3D('',#9721,#6217,#6218);
#5247=AXIS2_PLACEMENT_3D('',#9723,#6220,#6221);
#5248=AXIS2_PLACEMENT_3D('',#9725,#6222,#6223);
#5249=AXIS2_PLACEMENT_3D('',#9728,#6225,#6226);
#5250=AXIS2_PLACEMENT_3D('',#9729,#6227,#6228);
#5251=AXIS2_PLACEMENT_3D('',#9731,#6229,#6230);
#5252=AXIS2_PLACEMENT_3D('',#9732,#6231,#6232);
#5253=AXIS2_PLACEMENT_3D('',#9734,#6233,#6234);
#5254=AXIS2_PLACEMENT_3D('',#9736,#6236,#6237);
#5255=AXIS2_PLACEMENT_3D('',#9738,#6238,#6239);
#5256=AXIS2_PLACEMENT_3D('',#9741,#6241,#6242);
#5257=AXIS2_PLACEMENT_3D('',#9742,#6243,#6244);
#5258=AXIS2_PLACEMENT_3D('',#9743,#6245,#6246);
#5259=AXIS2_PLACEMENT_3D('',#9744,#6247,#6248);
#5260=AXIS2_PLACEMENT_3D('',#9745,#6249,#6250);
#5261=AXIS2_PLACEMENT_3D('',#9746,#6251,#6252);
#5262=AXIS2_PLACEMENT_3D('',#9749,#6253,#6254);
#5263=AXIS2_PLACEMENT_3D('',#9755,#6258,#6259);
#5264=AXIS2_PLACEMENT_3D('',#9761,#6263,#6264);
#5265=AXIS2_PLACEMENT_3D('',#9763,#6265,#6266);
#5266=AXIS2_PLACEMENT_3D('',#9767,#6269,#6270);
#5267=AXIS2_PLACEMENT_3D('',#9770,#6273,#6274);
#5268=AXIS2_PLACEMENT_3D('',#9771,#6275,#6276);
#5269=AXIS2_PLACEMENT_3D('',#9773,#6277,#6278);
#5270=AXIS2_PLACEMENT_3D('',#9775,#6279,#6280);
#5271=AXIS2_PLACEMENT_3D('',#9776,#6281,#6282);
#5272=AXIS2_PLACEMENT_3D('',#9778,#6283,#6284);
#5273=AXIS2_PLACEMENT_3D('',#9780,#6286,#6287);
#5274=AXIS2_PLACEMENT_3D('',#9782,#6288,#6289);
#5275=AXIS2_PLACEMENT_3D('',#9783,#6290,#6291);
#5276=AXIS2_PLACEMENT_3D('',#9785,#6292,#6293);
#5277=AXIS2_PLACEMENT_3D('',#9787,#6295,#6296);
#5278=AXIS2_PLACEMENT_3D('',#9789,#6297,#6298);
#5279=AXIS2_PLACEMENT_3D('',#9790,#6299,#6300);
#5280=AXIS2_PLACEMENT_3D('',#9792,#6301,#6302);
#5281=AXIS2_PLACEMENT_3D('',#9794,#6304,#6305);
#5282=AXIS2_PLACEMENT_3D('',#9796,#6306,#6307);
#5283=AXIS2_PLACEMENT_3D('',#9797,#6308,#6309);
#5284=AXIS2_PLACEMENT_3D('',#9799,#6310,#6311);
#5285=AXIS2_PLACEMENT_3D('',#9801,#6313,#6314);
#5286=AXIS2_PLACEMENT_3D('',#9803,#6315,#6316);
#5287=AXIS2_PLACEMENT_3D('',#9804,#6317,#6318);
#5288=AXIS2_PLACEMENT_3D('',#9806,#6319,#6320);
#5289=AXIS2_PLACEMENT_3D('',#9808,#6322,#6323);
#5290=AXIS2_PLACEMENT_3D('',#9810,#6324,#6325);
#5291=AXIS2_PLACEMENT_3D('',#9811,#6326,#6327);
#5292=AXIS2_PLACEMENT_3D('',#9813,#6329,#6330);
#5293=AXIS2_PLACEMENT_3D('',#9814,#6331,#6332);
#5294=AXIS2_PLACEMENT_3D('',#9817,#6333,#6334);
#5295=AXIS2_PLACEMENT_3D('',#9821,#6336,#6337);
#5296=AXIS2_PLACEMENT_3D('',#9823,#6339,#6340);
#5297=AXIS2_PLACEMENT_3D('',#9829,#6344,#6345);
#5298=AXIS2_PLACEMENT_3D('',#9831,#6346,#6347);
#5299=AXIS2_PLACEMENT_3D('',#9833,#6348,#6349);
#5300=AXIS2_PLACEMENT_3D('',#9835,#6351,#6352);
#5301=AXIS2_PLACEMENT_3D('',#9838,#6355,#6356);
#5302=AXIS2_PLACEMENT_3D('',#9840,#6357,#6358);
#5303=AXIS2_PLACEMENT_3D('',#9842,#6359,#6360);
#5304=AXIS2_PLACEMENT_3D('',#9843,#6361,#6362);
#5305=AXIS2_PLACEMENT_3D('',#9845,#6363,#6364);
#5306=AXIS2_PLACEMENT_3D('',#9847,#6366,#6367);
#5307=AXIS2_PLACEMENT_3D('',#9849,#6368,#6369);
#5308=AXIS2_PLACEMENT_3D('',#9850,#6370,#6371);
#5309=AXIS2_PLACEMENT_3D('',#9852,#6373,#6374);
#5310=AXIS2_PLACEMENT_3D('',#9853,#6375,#6376);
#5311=AXIS2_PLACEMENT_3D('',#9854,#6377,#6378);
#5312=AXIS2_PLACEMENT_3D('',#9855,#6379,#6380);
#5313=AXIS2_PLACEMENT_3D('',#9864,#6385,#6386);
#5314=AXIS2_PLACEMENT_3D('',#9870,#6390,#6391);
#5315=AXIS2_PLACEMENT_3D('',#9876,#6395,#6396);
#5316=AXIS2_PLACEMENT_3D('',#9882,#6400,#6401);
#5317=AXIS2_PLACEMENT_3D('',#9888,#6405,#6406);
#5318=AXIS2_PLACEMENT_3D('',#9891,#6409,#6410);
#5319=AXIS2_PLACEMENT_3D('',#9892,#6411,#6412);
#5320=AXIS2_PLACEMENT_3D('',#9893,#6413,#6414);
#5321=AXIS2_PLACEMENT_3D('',#9895,#6415,#6416);
#5322=AXIS2_PLACEMENT_3D('',#9896,#6417,#6418);
#5323=AXIS2_PLACEMENT_3D('',#9898,#6419,#6420);
#5324=AXIS2_PLACEMENT_3D('',#9899,#6421,#6422);
#5325=AXIS2_PLACEMENT_3D('',#9901,#6423,#6424);
#5326=AXIS2_PLACEMENT_3D('',#9903,#6426,#6427);
#5327=AXIS2_PLACEMENT_3D('',#9905,#6428,#6429);
#5328=AXIS2_PLACEMENT_3D('',#9907,#6431,#6432);
#5329=AXIS2_PLACEMENT_3D('',#9909,#6433,#6434);
#5330=AXIS2_PLACEMENT_3D('',#9911,#6436,#6437);
#5331=AXIS2_PLACEMENT_3D('',#9913,#6438,#6439);
#5332=AXIS2_PLACEMENT_3D('',#9914,#6440,#6441);
#5333=AXIS2_PLACEMENT_3D('',#9916,#6442,#6443);
#5334=AXIS2_PLACEMENT_3D('',#9918,#6445,#6446);
#5335=AXIS2_PLACEMENT_3D('',#9920,#6448,#6449);
#5336=AXIS2_PLACEMENT_3D('',#9921,#6450,#6451);
#5337=AXIS2_PLACEMENT_3D('',#9922,#6452,#6453);
#5338=AXIS2_PLACEMENT_3D('',#9924,#6454,#6455);
#5339=AXIS2_PLACEMENT_3D('',#9926,#6456,#6457);
#5340=AXIS2_PLACEMENT_3D('',#9927,#6458,#6459);
#5341=AXIS2_PLACEMENT_3D('',#9929,#6460,#6461);
#5342=AXIS2_PLACEMENT_3D('',#9931,#6462,#6463);
#5343=AXIS2_PLACEMENT_3D('',#9932,#6464,#6465);
#5344=AXIS2_PLACEMENT_3D('',#9934,#6467,#6468);
#5345=AXIS2_PLACEMENT_3D('',#9936,#6469,#6470);
#5346=AXIS2_PLACEMENT_3D('',#9938,#6471,#6472);
#5347=AXIS2_PLACEMENT_3D('',#9939,#6473,#6474);
#5348=AXIS2_PLACEMENT_3D('',#9941,#6476,#6477);
#5349=AXIS2_PLACEMENT_3D('',#9944,#6479,#6480);
#5350=AXIS2_PLACEMENT_3D('',#9945,#6481,#6482);
#5351=AXIS2_PLACEMENT_3D('',#9947,#6483,#6484);
#5352=AXIS2_PLACEMENT_3D('',#9949,#6486,#6487);
#5353=AXIS2_PLACEMENT_3D('',#9950,#6488,#6489);
#5354=AXIS2_PLACEMENT_3D('',#9951,#6490,#6491);
#5355=AXIS2_PLACEMENT_3D('',#9952,#6492,#6493);
#5356=AXIS2_PLACEMENT_3D('',#9954,#6494,#6495);
#5357=AXIS2_PLACEMENT_3D('',#9957,#6497,#6498);
#5358=AXIS2_PLACEMENT_3D('',#9958,#6499,#6500);
#5359=AXIS2_PLACEMENT_3D('',#9960,#6501,#6502);
#5360=AXIS2_PLACEMENT_3D('',#9963,#6504,#6505);
#5361=AXIS2_PLACEMENT_3D('',#9964,#6506,#6507);
#5362=AXIS2_PLACEMENT_3D('',#9965,#6508,#6509);
#5363=AXIS2_PLACEMENT_3D('',#9966,#6510,#6511);
#5364=AXIS2_PLACEMENT_3D('',#9967,#6512,#6513);
#5365=AXIS2_PLACEMENT_3D('',#9971,#6515,#6516);
#5366=AXIS2_PLACEMENT_3D('',#9972,#6517,#6518);
#5367=AXIS2_PLACEMENT_3D('',#9989,#6519,#6520);
#5368=AXIS2_PLACEMENT_3D('',#10046,#6522,#6523);
#5369=AXIS2_PLACEMENT_3D('',#10048,#6525,#6526);
#5370=AXIS2_PLACEMENT_3D('',#10050,#6527,#6528);
#5371=AXIS2_PLACEMENT_3D('',#10053,#6530,#6531);
#5372=AXIS2_PLACEMENT_3D('',#10054,#6532,#6533);
#5373=AXIS2_PLACEMENT_3D('',#10056,#6534,#6535);
#5374=AXIS2_PLACEMENT_3D('',#10059,#6537,#6538);
#5375=AXIS2_PLACEMENT_3D('',#10060,#6539,#6540);
#5376=AXIS2_PLACEMENT_3D('',#10061,#6541,#6542);
#5377=AXIS2_PLACEMENT_3D('',#10062,#6543,#6544);
#5378=AXIS2_PLACEMENT_3D('',#10063,#6545,#6546);
#5379=AXIS2_PLACEMENT_3D('',#10065,#6547,#6548);
#5380=AXIS2_PLACEMENT_3D('',#10066,#6549,#6550);
#5381=AXIS2_PLACEMENT_3D('',#10075,#6555,#6556);
#5382=AXIS2_PLACEMENT_3D('',#10081,#6560,#6561);
#5383=AXIS2_PLACEMENT_3D('',#10087,#6565,#6566);
#5384=AXIS2_PLACEMENT_3D('',#10093,#6570,#6571);
#5385=AXIS2_PLACEMENT_3D('',#10099,#6575,#6576);
#5386=AXIS2_PLACEMENT_3D('',#10102,#6579,#6580);
#5387=AXIS2_PLACEMENT_3D('',#10103,#6581,#6582);
#5388=AXIS2_PLACEMENT_3D('',#10105,#6583,#6584);
#5389=AXIS2_PLACEMENT_3D('',#10106,#6585,#6586);
#5390=AXIS2_PLACEMENT_3D('',#10108,#6587,#6588);
#5391=AXIS2_PLACEMENT_3D('',#10110,#6590,#6591);
#5392=AXIS2_PLACEMENT_3D('',#10112,#6593,#6594);
#5393=AXIS2_PLACEMENT_3D('',#10113,#6595,#6596);
#5394=AXIS2_PLACEMENT_3D('',#10114,#6597,#6598);
#5395=AXIS2_PLACEMENT_3D('',#10115,#6599,#6600);
#5396=AXIS2_PLACEMENT_3D('',#10116,#6601,#6602);
#5397=AXIS2_PLACEMENT_3D('',#10117,#6603,#6604);
#5398=AXIS2_PLACEMENT_3D('',#10118,#6605,#6606);
#5399=AXIS2_PLACEMENT_3D('',#10122,#6608,#6609);
#5400=AXIS2_PLACEMENT_3D('',#10123,#6610,#6611);
#5401=AXIS2_PLACEMENT_3D('',#10127,#6613,#6614);
#5402=AXIS2_PLACEMENT_3D('',#10128,#6615,#6616);
#5403=AXIS2_PLACEMENT_3D('',#10132,#6618,#6619);
#5404=AXIS2_PLACEMENT_3D('',#10134,#6621,#6622);
#5405=AXIS2_PLACEMENT_3D('',#10139,#6625,#6626);
#5406=AXIS2_PLACEMENT_3D('',#10140,#6627,#6628);
#5407=AXIS2_PLACEMENT_3D('',#10152,#6635,#6636);
#5408=AXIS2_PLACEMENT_3D('',#10153,#6637,#6638);
#5409=AXIS2_PLACEMENT_3D('',#10167,#6646,#6647);
#5410=AXIS2_PLACEMENT_3D('',#10169,#6648,#6649);
#5411=AXIS2_PLACEMENT_3D('',#10172,#6651,#6652);
#5412=AXIS2_PLACEMENT_3D('',#10173,#6653,#6654);
#5413=AXIS2_PLACEMENT_3D('',#10175,#6655,#6656);
#5414=AXIS2_PLACEMENT_3D('',#10178,#6658,#6659);
#5415=AXIS2_PLACEMENT_3D('',#10179,#6660,#6661);
#5416=AXIS2_PLACEMENT_3D('',#10183,#6663,#6664);
#5417=AXIS2_PLACEMENT_3D('',#10184,#6665,#6666);
#5418=AXIS2_PLACEMENT_3D('',#10185,#6667,#6668);
#5419=AXIS2_PLACEMENT_3D('',#10187,#6670,#6671);
#5420=AXIS2_PLACEMENT_3D('',#10191,#6674,#6675);
#5421=AXIS2_PLACEMENT_3D('',#10199,#6680,#6681);
#5422=AXIS2_PLACEMENT_3D('',#10200,#6682,#6683);
#5423=AXIS2_PLACEMENT_3D('',#10201,#6684,#6685);
#5424=AXIS2_PLACEMENT_3D('',#10202,#6686,#6687);
#5425=AXIS2_PLACEMENT_3D('',#10203,#6688,#6689);
#5426=AXIS2_PLACEMENT_3D('',#10205,#6691,#6692);
#5427=AXIS2_PLACEMENT_3D('',#10207,#6693,#6694);
#5428=AXIS2_PLACEMENT_3D('',#10209,#6696,#6697);
#5429=AXIS2_PLACEMENT_3D('',#10210,#6698,#6699);
#5430=AXIS2_PLACEMENT_3D('',#10211,#6700,#6701);
#5431=AXIS2_PLACEMENT_3D('',#10212,#6702,#6703);
#5432=AXIS2_PLACEMENT_3D('',#10214,#6704,#6705);
#5433=AXIS2_PLACEMENT_3D('',#10217,#6707,#6708);
#5434=AXIS2_PLACEMENT_3D('',#10218,#6709,#6710);
#5435=AXIS2_PLACEMENT_3D('',#10219,#6711,#6712);
#5436=AXIS2_PLACEMENT_3D('',#10221,#6713,#6714);
#5437=AXIS2_PLACEMENT_3D('',#10223,#6715,#6716);
#5438=AXIS2_PLACEMENT_3D('',#10224,#6717,#6718);
#5439=AXIS2_PLACEMENT_3D('',#10227,#6720,#6721);
#5440=AXIS2_PLACEMENT_3D('',#10228,#6722,#6723);
#5441=AXIS2_PLACEMENT_3D('',#10229,#6724,#6725);
#5442=AXIS2_PLACEMENT_3D('',#10231,#6726,#6727);
#5443=AXIS2_PLACEMENT_3D('',#10233,#6729,#6730);
#5444=AXIS2_PLACEMENT_3D('',#10234,#6731,#6732);
#5445=AXIS2_PLACEMENT_3D('',#10235,#6733,#6734);
#5446=AXIS2_PLACEMENT_3D('',#10237,#6735,#6736);
#5447=AXIS2_PLACEMENT_3D('',#10240,#6738,#6739);
#5448=AXIS2_PLACEMENT_3D('',#10241,#6740,#6741);
#5449=AXIS2_PLACEMENT_3D('',#10243,#6742,#6743);
#5450=AXIS2_PLACEMENT_3D('',#10246,#6745,#6746);
#5451=AXIS2_PLACEMENT_3D('',#10247,#6747,#6748);
#5452=AXIS2_PLACEMENT_3D('',#10248,#6749,#6750);
#5453=AXIS2_PLACEMENT_3D('',#10249,#6751,#6752);
#5454=AXIS2_PLACEMENT_3D('',#10250,#6753,#6754);
#5455=AXIS2_PLACEMENT_3D('',#10252,#6755,#6756);
#5456=AXIS2_PLACEMENT_3D('',#10255,#6758,#6759);
#5457=AXIS2_PLACEMENT_3D('',#10256,#6760,#6761);
#5458=AXIS2_PLACEMENT_3D('',#10258,#6762,#6763);
#5459=AXIS2_PLACEMENT_3D('',#10261,#6765,#6766);
#5460=AXIS2_PLACEMENT_3D('',#10262,#6767,#6768);
#5461=AXIS2_PLACEMENT_3D('',#10263,#6769,#6770);
#5462=AXIS2_PLACEMENT_3D('',#10264,#6771,#6772);
#5463=AXIS2_PLACEMENT_3D('',#10265,#6773,#6774);
#5464=AXIS2_PLACEMENT_3D('',#10267,#6775,#6776);
#5465=AXIS2_PLACEMENT_3D('',#10270,#6778,#6779);
#5466=AXIS2_PLACEMENT_3D('',#10271,#6780,#6781);
#5467=AXIS2_PLACEMENT_3D('',#10273,#6782,#6783);
#5468=AXIS2_PLACEMENT_3D('',#10276,#6785,#6786);
#5469=AXIS2_PLACEMENT_3D('',#10277,#6787,#6788);
#5470=AXIS2_PLACEMENT_3D('',#10278,#6789,#6790);
#5471=AXIS2_PLACEMENT_3D('',#10279,#6791,#6792);
#5472=AXIS2_PLACEMENT_3D('',#10280,#6793,#6794);
#5473=AXIS2_PLACEMENT_3D('',#10289,#6799,#6800);
#5474=AXIS2_PLACEMENT_3D('',#10295,#6804,#6805);
#5475=AXIS2_PLACEMENT_3D('',#10301,#6809,#6810);
#5476=AXIS2_PLACEMENT_3D('',#10307,#6814,#6815);
#5477=AXIS2_PLACEMENT_3D('',#10313,#6819,#6820);
#5478=AXIS2_PLACEMENT_3D('',#10316,#6823,#6824);
#5479=AXIS2_PLACEMENT_3D('',#10317,#6825,#6826);
#5480=AXIS2_PLACEMENT_3D('',#10318,#6827,#6828);
#5481=AXIS2_PLACEMENT_3D('',#10320,#6829,#6830);
#5482=AXIS2_PLACEMENT_3D('',#10321,#6831,#6832);
#5483=AXIS2_PLACEMENT_3D('',#10323,#6833,#6834);
#5484=AXIS2_PLACEMENT_3D('',#10324,#6835,#6836);
#5485=AXIS2_PLACEMENT_3D('',#10326,#6837,#6838);
#5486=AXIS2_PLACEMENT_3D('',#10328,#6840,#6841);
#5487=AXIS2_PLACEMENT_3D('',#10330,#6842,#6843);
#5488=AXIS2_PLACEMENT_3D('',#10332,#6845,#6846);
#5489=AXIS2_PLACEMENT_3D('',#10334,#6847,#6848);
#5490=AXIS2_PLACEMENT_3D('',#10336,#6850,#6851);
#5491=AXIS2_PLACEMENT_3D('',#10338,#6852,#6853);
#5492=AXIS2_PLACEMENT_3D('',#10339,#6854,#6855);
#5493=AXIS2_PLACEMENT_3D('',#10341,#6856,#6857);
#5494=AXIS2_PLACEMENT_3D('',#10343,#6859,#6860);
#5495=AXIS2_PLACEMENT_3D('',#10345,#6862,#6863);
#5496=AXIS2_PLACEMENT_3D('',#10346,#6864,#6865);
#5497=AXIS2_PLACEMENT_3D('',#10347,#6866,#6867);
#5498=AXIS2_PLACEMENT_3D('',#10348,#6868,#6869);
#5499=AXIS2_PLACEMENT_3D('',#10349,#6870,#6871);
#5500=AXIS2_PLACEMENT_3D('',#10350,#6872,#6873);
#5501=AXIS2_PLACEMENT_3D('',#10351,#6874,#6875);
#5502=AXIS2_PLACEMENT_3D('',#10352,#6876,#6877);
#5503=AXIS2_PLACEMENT_3D('',#10353,#6878,#6879);
#5504=AXIS2_PLACEMENT_3D('',#10354,#6880,#6881);
#5505=AXIS2_PLACEMENT_3D('',#10357,#6882,#6883);
#5506=AXIS2_PLACEMENT_3D('',#10358,#6884,#6885);
#5507=AXIS2_PLACEMENT_3D('',#10360,#6886,#6887);
#5508=AXIS2_PLACEMENT_3D('',#10362,#6888,#6889);
#5509=AXIS2_PLACEMENT_3D('',#10363,#6890,#6891);
#5510=AXIS2_PLACEMENT_3D('',#10364,#6892,#6893);
#5511=AXIS2_PLACEMENT_3D('',#10367,#6895,#6896);
#5512=AXIS2_PLACEMENT_3D('',#10368,#6897,#6898);
#5513=AXIS2_PLACEMENT_3D('',#10370,#6899,#6900);
#5514=AXIS2_PLACEMENT_3D('',#10373,#6902,#6903);
#5515=AXIS2_PLACEMENT_3D('',#10374,#6904,#6905);
#5516=AXIS2_PLACEMENT_3D('',#10377,#6907,#6908);
#5517=AXIS2_PLACEMENT_3D('',#10378,#6909,#6910);
#5518=AXIS2_PLACEMENT_3D('',#10379,#6911,#6912);
#5519=AXIS2_PLACEMENT_3D('',#10381,#6913,#6914);
#5520=AXIS2_PLACEMENT_3D('',#10383,#6916,#6917);
#5521=AXIS2_PLACEMENT_3D('',#10385,#6918,#6919);
#5522=AXIS2_PLACEMENT_3D('',#10386,#6920,#6921);
#5523=AXIS2_PLACEMENT_3D('',#10388,#6923,#6924);
#5524=AXIS2_PLACEMENT_3D('',#10389,#6925,#6926);
#5525=AXIS2_PLACEMENT_3D('',#10392,#6927,#6928);
#5526=AXIS2_PLACEMENT_3D('',#10393,#6929,#6930);
#5527=AXIS2_PLACEMENT_3D('',#10395,#6931,#6932);
#5528=AXIS2_PLACEMENT_3D('',#10397,#6933,#6934);
#5529=AXIS2_PLACEMENT_3D('',#10398,#6935,#6936);
#5530=AXIS2_PLACEMENT_3D('',#10399,#6937,#6938);
#5531=AXIS2_PLACEMENT_3D('',#10401,#6939,#6940);
#5532=AXIS2_PLACEMENT_3D('',#10403,#6942,#6943);
#5533=AXIS2_PLACEMENT_3D('',#10405,#6944,#6945);
#5534=AXIS2_PLACEMENT_3D('',#10407,#6946,#6947);
#5535=AXIS2_PLACEMENT_3D('',#10408,#6948,#6949);
#5536=AXIS2_PLACEMENT_3D('',#10410,#6950,#6951);
#5537=AXIS2_PLACEMENT_3D('',#10412,#6953,#6954);
#5538=AXIS2_PLACEMENT_3D('',#10414,#6955,#6956);
#5539=AXIS2_PLACEMENT_3D('',#10416,#6958,#6959);
#5540=AXIS2_PLACEMENT_3D('',#10418,#6960,#6961);
#5541=AXIS2_PLACEMENT_3D('',#10420,#6963,#6964);
#5542=AXIS2_PLACEMENT_3D('',#10421,#6965,#6966);
#5543=AXIS2_PLACEMENT_3D('',#10423,#6968,#6969);
#5544=AXIS2_PLACEMENT_3D('',#10424,#6970,#6971);
#5545=AXIS2_PLACEMENT_3D('',#10427,#6972,#6973);
#5546=AXIS2_PLACEMENT_3D('',#10428,#6974,#6975);
#5547=AXIS2_PLACEMENT_3D('',#10431,#6976,#6977);
#5548=AXIS2_PLACEMENT_3D('',#10432,#6978,#6979);
#5549=AXIS2_PLACEMENT_3D('',#10435,#6980,#6981);
#5550=AXIS2_PLACEMENT_3D('',#10436,#6982,#6983);
#5551=AXIS2_PLACEMENT_3D('',#10439,#6984,#6985);
#5552=AXIS2_PLACEMENT_3D('',#10440,#6986,#6987);
#5553=AXIS2_PLACEMENT_3D('',#10443,#6988,#6989);
#5554=AXIS2_PLACEMENT_3D('',#10444,#6990,#6991);
#5555=AXIS2_PLACEMENT_3D('',#10447,#6992,#6993);
#5556=AXIS2_PLACEMENT_3D('',#10448,#6994,#6995);
#5557=AXIS2_PLACEMENT_3D('',#10451,#6996,#6997);
#5558=AXIS2_PLACEMENT_3D('',#10452,#6998,#6999);
#5559=AXIS2_PLACEMENT_3D('',#10455,#7000,#7001);
#5560=AXIS2_PLACEMENT_3D('',#10456,#7002,#7003);
#5561=AXIS2_PLACEMENT_3D('',#10457,#7004,#7005);
#5562=AXIS2_PLACEMENT_3D('',#10483,#7006,#7007);
#5563=AXIS2_PLACEMENT_3D('',#10507,#7008,#7009);
#5564=AXIS2_PLACEMENT_3D('',#10508,#7010,#7011);
#5565=AXIS2_PLACEMENT_3D('',#10510,#7012,#7013);
#5566=AXIS2_PLACEMENT_3D('',#10535,#7014,#7015);
#5567=AXIS2_PLACEMENT_3D('',#10560,#7016,#7017);
#5568=AXIS2_PLACEMENT_3D('',#10576,#7019,#7020);
#5569=AXIS2_PLACEMENT_3D('',#10591,#7021,#7022);
#5570=AXIS2_PLACEMENT_3D('',#10616,#7023,#7024);
#5571=AXIS2_PLACEMENT_3D('',#10641,#7025,#7026);
#5572=AXIS2_PLACEMENT_3D('',#10666,#7027,#7028);
#5573=AXIS2_PLACEMENT_3D('',#10690,#7029,#7030);
#5574=AXIS2_PLACEMENT_3D('',#10691,#7031,#7032);
#5575=AXIS2_PLACEMENT_3D('',#10693,#7033,#7034);
#5576=AXIS2_PLACEMENT_3D('',#10694,#7035,#7036);
#5577=AXIS2_PLACEMENT_3D('',#10695,#7037,#7038);
#5578=AXIS2_PLACEMENT_3D('',#10719,#7039,#7040);
#5579=AXIS2_PLACEMENT_3D('',#10720,#7041,#7042);
#5580=AXIS2_PLACEMENT_3D('',#10722,#7043,#7044);
#5581=AXIS2_PLACEMENT_3D('',#10723,#7045,#7046);
#5582=AXIS2_PLACEMENT_3D('',#10724,#7047,#7048);
#5583=AXIS2_PLACEMENT_3D('',#10748,#7049,#7050);
#5584=AXIS2_PLACEMENT_3D('',#10749,#7051,#7052);
#5585=AXIS2_PLACEMENT_3D('',#10751,#7053,#7054);
#5586=AXIS2_PLACEMENT_3D('',#10752,#7055,#7056);
#5587=AXIS2_PLACEMENT_3D('',#10753,#7057,#7058);
#5588=AXIS2_PLACEMENT_3D('',#10768,#7059,#7060);
#5589=AXIS2_PLACEMENT_3D('',#10781,#7061,#7062);
#5590=AXIS2_PLACEMENT_3D('',#10783,#7063,#7064);
#5591=AXIS2_PLACEMENT_3D('',#10784,#7065,#7066);
#5592=AXIS2_PLACEMENT_3D('',#10785,#7067,#7068);
#5593=AXIS2_PLACEMENT_3D('',#10809,#7069,#7070);
#5594=AXIS2_PLACEMENT_3D('',#10810,#7071,#7072);
#5595=AXIS2_PLACEMENT_3D('',#10812,#7073,#7074);
#5596=AXIS2_PLACEMENT_3D('',#10813,#7075,#7076);
#5597=AXIS2_PLACEMENT_3D('',#10814,#7077,#7078);
#5598=AXIS2_PLACEMENT_3D('',#10838,#7079,#7080);
#5599=AXIS2_PLACEMENT_3D('',#10839,#7081,#7082);
#5600=AXIS2_PLACEMENT_3D('',#10841,#7083,#7084);
#5601=AXIS2_PLACEMENT_3D('',#10842,#7085,#7086);
#5602=AXIS2_PLACEMENT_3D('',#10843,#7087,#7088);
#5603=AXIS2_PLACEMENT_3D('',#10867,#7089,#7090);
#5604=AXIS2_PLACEMENT_3D('',#10868,#7091,#7092);
#5605=AXIS2_PLACEMENT_3D('',#10870,#7093,#7094);
#5606=AXIS2_PLACEMENT_3D('',#10873,#7096,#7097);
#5607=AXIS2_PLACEMENT_3D('',#10897,#7098,#7099);
#5608=AXIS2_PLACEMENT_3D('',#10898,#7100,#7101);
#5609=AXIS2_PLACEMENT_3D('',#10899,#7102,#7103);
#5610=AXIS2_PLACEMENT_3D('',#10900,#7104,#7105);
#5611=AXIS2_PLACEMENT_3D('',#10901,#7106,#7107);
#5612=AXIS2_PLACEMENT_3D('',#10902,#7108,#7109);
#5613=AXIS2_PLACEMENT_3D('',#10903,#7110,#7111);
#5614=AXIS2_PLACEMENT_3D('',#10904,#7112,#7113);
#5615=AXIS2_PLACEMENT_3D('',#10905,#7114,#7115);
#5616=AXIS2_PLACEMENT_3D('',#10907,#7116,#7117);
#5617=AXIS2_PLACEMENT_3D('',#10909,#7118,#7119);
#5618=AXIS2_PLACEMENT_3D('',#10910,#7120,#7121);
#5619=AXIS2_PLACEMENT_3D('',#10912,#7122,#7123);
#5620=AXIS2_PLACEMENT_3D('',#10914,#7125,#7126);
#5621=AXIS2_PLACEMENT_3D('',#10916,#7127,#7128);
#5622=AXIS2_PLACEMENT_3D('',#10917,#7129,#7130);
#5623=AXIS2_PLACEMENT_3D('',#10919,#7132,#7133);
#5624=AXIS2_PLACEMENT_3D('',#10921,#7134,#7135);
#5625=AXIS2_PLACEMENT_3D('',#10923,#7136,#7137);
#5626=AXIS2_PLACEMENT_3D('',#10924,#7138,#7139);
#5627=AXIS2_PLACEMENT_3D('',#10926,#7140,#7141);
#5628=AXIS2_PLACEMENT_3D('',#10928,#7143,#7144);
#5629=AXIS2_PLACEMENT_3D('',#10930,#7145,#7146);
#5630=AXIS2_PLACEMENT_3D('',#10931,#7147,#7148);
#5631=AXIS2_PLACEMENT_3D('',#10933,#7150,#7151);
#5632=AXIS2_PLACEMENT_3D('',#10934,#7152,#7153);
#5633=AXIS2_PLACEMENT_3D('',#10935,#7154,#7155);
#5634=AXIS2_PLACEMENT_3D('',#10936,#7156,#7157);
#5635=AXIS2_PLACEMENT_3D('',#10937,#7158,#7159);
#5636=AXIS2_PLACEMENT_3D('',#10938,#7160,#7161);
#5637=AXIS2_PLACEMENT_3D('',#10939,#7162,#7163);
#5638=AXIS2_PLACEMENT_3D('',#10940,#7164,#7165);
#5639=AXIS2_PLACEMENT_3D('',#10941,#7166,#7167);
#5640=AXIS2_PLACEMENT_3D('',#10942,#7168,#7169);
#5641=AXIS2_PLACEMENT_3D('',#10943,#7170,#7171);
#5642=AXIS2_PLACEMENT_3D('',#10944,#7172,#7173);
#5643=AXIS2_PLACEMENT_3D('',#10945,#7174,#7175);
#5644=AXIS2_PLACEMENT_3D('',#10946,#7176,#7177);
#5645=AXIS2_PLACEMENT_3D('',#10947,#7178,#7179);
#5646=AXIS2_PLACEMENT_3D('',#10948,#7180,#7181);
#5647=AXIS2_PLACEMENT_3D('',#10949,#7182,#7183);
#5648=AXIS2_PLACEMENT_3D('',#10950,#7184,#7185);
#5649=AXIS2_PLACEMENT_3D('',#10951,#7186,#7187);
#5650=AXIS2_PLACEMENT_3D('',#10952,#7188,#7189);
#5651=AXIS2_PLACEMENT_3D('',#10953,#7190,#7191);
#5652=AXIS2_PLACEMENT_3D('',#10954,#7192,#7193);
#5653=AXIS2_PLACEMENT_3D('',#10955,#7194,#7195);
#5654=AXIS2_PLACEMENT_3D('',#10956,#7196,#7197);
#5655=AXIS2_PLACEMENT_3D('',#10957,#7198,#7199);
#5656=AXIS2_PLACEMENT_3D('',#10958,#7200,#7201);
#5657=AXIS2_PLACEMENT_3D('',#10959,#7202,#7203);
#5658=AXIS2_PLACEMENT_3D('',#10960,#7204,#7205);
#5659=AXIS2_PLACEMENT_3D('',#10961,#7206,#7207);
#5660=AXIS2_PLACEMENT_3D('',#10962,#7208,#7209);
#5661=AXIS2_PLACEMENT_3D('',#10963,#7210,#7211);
#5662=AXIS2_PLACEMENT_3D('',#10964,#7212,#7213);
#5663=AXIS2_PLACEMENT_3D('',#10965,#7214,#7215);
#5664=AXIS2_PLACEMENT_3D('',#10966,#7216,#7217);
#5665=AXIS2_PLACEMENT_3D('',#10967,#7218,#7219);
#5666=AXIS2_PLACEMENT_3D('',#10968,#7220,#7221);
#5667=AXIS2_PLACEMENT_3D('',#10969,#7222,#7223);
#5668=DIRECTION('axis',(0.,0.,1.));
#5669=DIRECTION('refdir',(1.,0.,0.));
#5670=DIRECTION('axis',(0.,0.,1.));
#5671=DIRECTION('refdir',(1.,0.,0.));
#5672=DIRECTION('axis',(0.,0.,1.));
#5673=DIRECTION('refdir',(1.,0.,0.));
#5674=DIRECTION('center_axis',(0.,0.,1.));
#5675=DIRECTION('ref_axis',(1.,0.,0.));
#5676=DIRECTION('center_axis',(0.,0.,1.));
#5677=DIRECTION('ref_axis',(1.,0.,0.));
#5678=DIRECTION('',(0.,0.,1.));
#5679=DIRECTION('center_axis',(0.,0.,-1.));
#5680=DIRECTION('ref_axis',(1.,0.,0.));
#5681=DIRECTION('center_axis',(0.,0.,1.));
#5682=DIRECTION('ref_axis',(1.,0.,0.));
#5683=DIRECTION('center_axis',(0.,0.,1.));
#5684=DIRECTION('ref_axis',(1.,0.,0.));
#5685=DIRECTION('',(0.,0.,1.));
#5686=DIRECTION('center_axis',(0.,0.,-1.));
#5687=DIRECTION('ref_axis',(1.,0.,0.));
#5688=DIRECTION('center_axis',(0.,0.,1.));
#5689=DIRECTION('ref_axis',(1.,0.,0.));
#5690=DIRECTION('center_axis',(0.,0.,1.));
#5691=DIRECTION('ref_axis',(1.,0.,0.));
#5692=DIRECTION('',(0.,0.,1.));
#5693=DIRECTION('center_axis',(0.,0.,-1.));
#5694=DIRECTION('ref_axis',(1.,0.,0.));
#5695=DIRECTION('center_axis',(0.,0.,1.));
#5696=DIRECTION('ref_axis',(1.,0.,0.));
#5697=DIRECTION('center_axis',(0.,0.,1.));
#5698=DIRECTION('ref_axis',(1.,0.,0.));
#5699=DIRECTION('',(0.,0.,1.));
#5700=DIRECTION('center_axis',(0.,0.,-1.));
#5701=DIRECTION('ref_axis',(1.,0.,0.));
#5702=DIRECTION('center_axis',(0.,0.,1.));
#5703=DIRECTION('ref_axis',(1.,0.,0.));
#5704=DIRECTION('center_axis',(0.,0.,1.));
#5705=DIRECTION('ref_axis',(1.,0.,0.));
#5706=DIRECTION('',(0.,0.,1.));
#5707=DIRECTION('center_axis',(0.,0.,-1.));
#5708=DIRECTION('ref_axis',(1.,0.,0.));
#5709=DIRECTION('center_axis',(0.,0.,1.));
#5710=DIRECTION('ref_axis',(1.,0.,0.));
#5711=DIRECTION('center_axis',(0.,0.,1.));
#5712=DIRECTION('ref_axis',(1.,0.,0.));
#5713=DIRECTION('',(0.,0.,1.));
#5714=DIRECTION('center_axis',(0.,0.,-1.));
#5715=DIRECTION('ref_axis',(1.,0.,0.));
#5716=DIRECTION('center_axis',(0.,1.,0.));
#5717=DIRECTION('ref_axis',(-1.,0.,0.));
#5718=DIRECTION('',(-1.,0.,0.));
#5719=DIRECTION('',(0.,0.,1.));
#5720=DIRECTION('',(-1.,0.,0.));
#5721=DIRECTION('',(0.,0.,1.));
#5722=DIRECTION('center_axis',(1.,0.,0.));
#5723=DIRECTION('ref_axis',(0.,1.,0.));
#5724=DIRECTION('',(0.,1.,0.));
#5725=DIRECTION('',(0.,1.,0.));
#5726=DIRECTION('',(0.,0.,1.));
#5727=DIRECTION('center_axis',(0.,-1.,0.));
#5728=DIRECTION('ref_axis',(1.,0.,0.));
#5729=DIRECTION('',(1.,0.,0.));
#5730=DIRECTION('',(1.,0.,0.));
#5731=DIRECTION('',(0.,0.,1.));
#5732=DIRECTION('center_axis',(-1.,0.,0.));
#5733=DIRECTION('ref_axis',(0.,-1.,0.));
#5734=DIRECTION('',(0.,-1.,0.));
#5735=DIRECTION('',(0.,-1.,0.));
#5736=DIRECTION('center_axis',(0.,0.,1.));
#5737=DIRECTION('ref_axis',(1.,0.,0.));
#5738=DIRECTION('center_axis',(0.,0.,1.));
#5739=DIRECTION('ref_axis',(1.,0.,0.));
#5740=DIRECTION('axis',(0.,0.,1.));
#5741=DIRECTION('refdir',(1.,0.,0.));
#5742=DIRECTION('center_axis',(0.,0.,1.));
#5743=DIRECTION('ref_axis',(1.,0.,0.));
#5744=DIRECTION('',(0.,-1.,0.));
#5745=DIRECTION('',(1.,0.,0.));
#5746=DIRECTION('',(0.,1.,0.));
#5747=DIRECTION('',(-1.,0.,0.));
#5748=DIRECTION('center_axis',(0.,0.,-1.));
#5749=DIRECTION('ref_axis',(1.,0.,0.));
#5750=DIRECTION('center_axis',(0.,0.,-1.));
#5751=DIRECTION('ref_axis',(1.,0.,0.));
#5752=DIRECTION('center_axis',(0.,1.,0.));
#5753=DIRECTION('ref_axis',(0.,0.,1.));
#5754=DIRECTION('',(-1.,0.,0.));
#5755=DIRECTION('',(0.,0.,1.));
#5756=DIRECTION('',(0.,0.,1.));
#5757=DIRECTION('center_axis',(0.,-1.,0.));
#5758=DIRECTION('ref_axis',(0.,0.,-1.));
#5759=DIRECTION('',(1.,0.,0.));
#5760=DIRECTION('',(0.,0.,1.));
#5761=DIRECTION('',(0.,0.,1.));
#5762=DIRECTION('center_axis',(1.,0.,0.));
#5763=DIRECTION('ref_axis',(0.,0.,-1.));
#5764=DIRECTION('center_axis',(1.,0.,0.));
#5765=DIRECTION('ref_axis',(0.,0.,-1.));
#5766=DIRECTION('',(1.,0.,0.));
#5767=DIRECTION('center_axis',(1.,0.,0.));
#5768=DIRECTION('ref_axis',(0.,0.,-1.));
#5769=DIRECTION('',(1.,0.,0.));
#5770=DIRECTION('center_axis',(-1.,0.,0.));
#5771=DIRECTION('ref_axis',(0.,0.,-1.));
#5772=DIRECTION('center_axis',(1.,0.,0.));
#5773=DIRECTION('ref_axis',(0.,0.,-1.));
#5774=DIRECTION('center_axis',(1.,0.,0.));
#5775=DIRECTION('ref_axis',(0.,0.,-1.));
#5776=DIRECTION('',(1.,0.,0.));
#5777=DIRECTION('center_axis',(1.,0.,0.));
#5778=DIRECTION('ref_axis',(0.,0.,-1.));
#5779=DIRECTION('',(1.,0.,0.));
#5780=DIRECTION('center_axis',(-1.,0.,0.));
#5781=DIRECTION('ref_axis',(0.,0.,-1.));
#5782=DIRECTION('center_axis',(1.,0.,0.));
#5783=DIRECTION('ref_axis',(0.,0.,-1.));
#5784=DIRECTION('center_axis',(1.,0.,0.));
#5785=DIRECTION('ref_axis',(0.,0.,-1.));
#5786=DIRECTION('',(1.,0.,0.));
#5787=DIRECTION('center_axis',(1.,0.,0.));
#5788=DIRECTION('ref_axis',(0.,0.,-1.));
#5789=DIRECTION('',(1.,0.,0.));
#5790=DIRECTION('center_axis',(-1.,0.,0.));
#5791=DIRECTION('ref_axis',(0.,0.,-1.));
#5792=DIRECTION('center_axis',(1.,0.,0.));
#5793=DIRECTION('ref_axis',(0.,0.,-1.));
#5794=DIRECTION('center_axis',(1.,0.,0.));
#5795=DIRECTION('ref_axis',(0.,0.,-1.));
#5796=DIRECTION('',(1.,0.,0.));
#5797=DIRECTION('center_axis',(1.,0.,0.));
#5798=DIRECTION('ref_axis',(0.,0.,-1.));
#5799=DIRECTION('',(1.,0.,0.));
#5800=DIRECTION('center_axis',(-1.,0.,0.));
#5801=DIRECTION('ref_axis',(0.,0.,-1.));
#5802=DIRECTION('center_axis',(0.,0.,1.));
#5803=DIRECTION('ref_axis',(1.,0.,0.));
#5804=DIRECTION('center_axis',(0.,0.,1.));
#5805=DIRECTION('ref_axis',(1.,0.,0.));
#5806=DIRECTION('',(0.,0.,1.));
#5807=DIRECTION('center_axis',(0.,0.,1.));
#5808=DIRECTION('ref_axis',(1.,0.,0.));
#5809=DIRECTION('center_axis',(0.,0.,1.));
#5810=DIRECTION('ref_axis',(1.,0.,0.));
#5811=DIRECTION('center_axis',(0.,0.,1.));
#5812=DIRECTION('ref_axis',(1.,0.,0.));
#5813=DIRECTION('center_axis',(0.,0.,1.));
#5814=DIRECTION('ref_axis',(1.,0.,0.));
#5815=DIRECTION('',(0.,0.,1.));
#5816=DIRECTION('center_axis',(0.,0.,1.));
#5817=DIRECTION('ref_axis',(1.,0.,0.));
#5818=DIRECTION('center_axis',(0.,0.,1.));
#5819=DIRECTION('ref_axis',(1.,0.,0.));
#5820=DIRECTION('',(0.,0.,1.));
#5821=DIRECTION('center_axis',(0.,0.,1.));
#5822=DIRECTION('ref_axis',(1.,0.,0.));
#5823=DIRECTION('center_axis',(0.,0.,1.));
#5824=DIRECTION('ref_axis',(1.,0.,0.));
#5825=DIRECTION('center_axis',(0.,0.,1.));
#5826=DIRECTION('ref_axis',(1.,0.,0.));
#5827=DIRECTION('center_axis',(0.,0.,1.));
#5828=DIRECTION('ref_axis',(1.,0.,0.));
#5829=DIRECTION('',(0.,0.,1.));
#5830=DIRECTION('center_axis',(1.,0.,0.));
#5831=DIRECTION('ref_axis',(0.,0.,-1.));
#5832=DIRECTION('center_axis',(1.,0.,0.));
#5833=DIRECTION('ref_axis',(0.,0.,-1.));
#5834=DIRECTION('',(1.,0.,0.));
#5835=DIRECTION('center_axis',(-1.,0.,0.));
#5836=DIRECTION('ref_axis',(0.,0.,-1.));
#5837=DIRECTION('center_axis',(1.,0.,0.));
#5838=DIRECTION('ref_axis',(0.,1.,0.));
#5839=DIRECTION('',(0.,-1.,0.));
#5840=DIRECTION('center_axis',(-1.,0.,0.));
#5841=DIRECTION('ref_axis',(0.,-1.,0.));
#5842=DIRECTION('',(0.,-1.,0.));
#5843=DIRECTION('center_axis',(0.,0.,1.));
#5844=DIRECTION('ref_axis',(1.,0.,0.));
#5845=DIRECTION('axis',(0.,0.,1.));
#5846=DIRECTION('refdir',(1.,0.,0.));
#5847=DIRECTION('center_axis',(1.,0.,0.));
#5848=DIRECTION('ref_axis',(0.,-0.707106781186549,0.707106781186546));
#5849=DIRECTION('',(1.,0.,0.));
#5850=DIRECTION('center_axis',(1.,0.,0.));
#5851=DIRECTION('ref_axis',(0.,0.,-1.));
#5852=DIRECTION('',(-1.,0.,0.));
#5853=DIRECTION('center_axis',(-1.,0.,0.));
#5854=DIRECTION('ref_axis',(0.,0.,-1.));
#5855=DIRECTION('center_axis',(1.,0.,0.));
#5856=DIRECTION('ref_axis',(0.,0.707106781186548,-0.707106781186547));
#5857=DIRECTION('',(1.,0.,0.));
#5858=DIRECTION('center_axis',(1.,0.,0.));
#5859=DIRECTION('ref_axis',(0.,0.,-1.));
#5860=DIRECTION('',(-1.,0.,0.));
#5861=DIRECTION('center_axis',(-1.,0.,0.));
#5862=DIRECTION('ref_axis',(0.,0.,-1.));
#5863=DIRECTION('center_axis',(1.,0.,0.));
#5864=DIRECTION('ref_axis',(0.,0.707106781186549,0.707106781186546));
#5865=DIRECTION('',(1.,0.,0.));
#5866=DIRECTION('center_axis',(1.,0.,0.));
#5867=DIRECTION('ref_axis',(0.,0.,-1.));
#5868=DIRECTION('',(-1.,0.,0.));
#5869=DIRECTION('center_axis',(-1.,0.,0.));
#5870=DIRECTION('ref_axis',(0.,0.,-1.));
#5871=DIRECTION('center_axis',(1.,0.,0.));
#5872=DIRECTION('ref_axis',(0.,-0.707106781186547,-0.707106781186548));
#5873=DIRECTION('',(1.,0.,0.));
#5874=DIRECTION('center_axis',(1.,0.,0.));
#5875=DIRECTION('ref_axis',(0.,0.,-1.));
#5876=DIRECTION('',(-1.,0.,0.));
#5877=DIRECTION('center_axis',(-1.,0.,0.));
#5878=DIRECTION('ref_axis',(0.,0.,-1.));
#5879=DIRECTION('center_axis',(1.,0.,0.));
#5880=DIRECTION('ref_axis',(0.,0.,-1.));
#5881=DIRECTION('center_axis',(1.,0.,0.));
#5882=DIRECTION('ref_axis',(0.,0.,-1.));
#5883=DIRECTION('center_axis',(1.,0.,0.));
#5884=DIRECTION('ref_axis',(0.,0.,-1.));
#5885=DIRECTION('center_axis',(1.,0.,0.));
#5886=DIRECTION('ref_axis',(0.,0.,-1.));
#5887=DIRECTION('center_axis',(1.,0.,0.));
#5888=DIRECTION('ref_axis',(0.,0.,-1.));
#5889=DIRECTION('center_axis',(-1.,0.,0.));
#5890=DIRECTION('ref_axis',(0.,0.,-1.));
#5891=DIRECTION('center_axis',(1.,0.,0.));
#5892=DIRECTION('ref_axis',(0.,-1.22464679914735E-16,1.));
#5893=DIRECTION('center_axis',(1.,0.,0.));
#5894=DIRECTION('ref_axis',(0.,0.,-1.));
#5895=DIRECTION('center_axis',(1.,0.,0.));
#5896=DIRECTION('ref_axis',(0.,0.,-1.));
#5897=DIRECTION('center_axis',(1.,0.,0.));
#5898=DIRECTION('ref_axis',(0.,0.,-1.));
#5899=DIRECTION('center_axis',(1.,0.,0.));
#5900=DIRECTION('ref_axis',(0.,0.,-1.));
#5901=DIRECTION('center_axis',(1.,0.,0.));
#5902=DIRECTION('ref_axis',(0.,0.,-1.));
#5903=DIRECTION('center_axis',(1.,0.,0.));
#5904=DIRECTION('ref_axis',(0.,0.,-1.));
#5905=DIRECTION('center_axis',(1.,0.,0.));
#5906=DIRECTION('ref_axis',(0.,0.,-1.));
#5907=DIRECTION('center_axis',(1.,0.,0.));
#5908=DIRECTION('ref_axis',(0.,0.,-1.));
#5909=DIRECTION('center_axis',(-1.,0.,0.));
#5910=DIRECTION('ref_axis',(0.,0.,-1.));
#5911=DIRECTION('',(-1.,0.,0.));
#5912=DIRECTION('center_axis',(1.,0.,0.));
#5913=DIRECTION('ref_axis',(0.,0.,-1.));
#5914=DIRECTION('axis',(0.,0.,1.));
#5915=DIRECTION('refdir',(1.,0.,0.));
#5916=DIRECTION('center_axis',(1.,0.,0.));
#5917=DIRECTION('ref_axis',(0.,-0.707106781186549,0.707106781186546));
#5918=DIRECTION('',(1.,0.,0.));
#5919=DIRECTION('center_axis',(1.,0.,0.));
#5920=DIRECTION('ref_axis',(0.,0.,-1.));
#5921=DIRECTION('',(-1.,0.,0.));
#5922=DIRECTION('center_axis',(-1.,0.,0.));
#5923=DIRECTION('ref_axis',(0.,0.,-1.));
#5924=DIRECTION('center_axis',(1.,0.,0.));
#5925=DIRECTION('ref_axis',(0.,0.707106781186548,-0.707106781186547));
#5926=DIRECTION('',(1.,0.,0.));
#5927=DIRECTION('center_axis',(1.,0.,0.));
#5928=DIRECTION('ref_axis',(0.,0.,-1.));
#5929=DIRECTION('',(-1.,0.,0.));
#5930=DIRECTION('center_axis',(-1.,0.,0.));
#5931=DIRECTION('ref_axis',(0.,0.,-1.));
#5932=DIRECTION('center_axis',(1.,0.,0.));
#5933=DIRECTION('ref_axis',(0.,0.707106781186549,0.707106781186546));
#5934=DIRECTION('',(1.,0.,0.));
#5935=DIRECTION('center_axis',(1.,0.,0.));
#5936=DIRECTION('ref_axis',(0.,0.,-1.));
#5937=DIRECTION('',(-1.,0.,0.));
#5938=DIRECTION('center_axis',(-1.,0.,0.));
#5939=DIRECTION('ref_axis',(0.,0.,-1.));
#5940=DIRECTION('center_axis',(1.,0.,0.));
#5941=DIRECTION('ref_axis',(0.,-0.707106781186547,-0.707106781186548));
#5942=DIRECTION('',(1.,0.,0.));
#5943=DIRECTION('center_axis',(1.,0.,0.));
#5944=DIRECTION('ref_axis',(0.,0.,-1.));
#5945=DIRECTION('',(-1.,0.,0.));
#5946=DIRECTION('center_axis',(-1.,0.,0.));
#5947=DIRECTION('ref_axis',(0.,0.,-1.));
#5948=DIRECTION('center_axis',(1.,0.,0.));
#5949=DIRECTION('ref_axis',(0.,0.,-1.));
#5950=DIRECTION('center_axis',(1.,0.,0.));
#5951=DIRECTION('ref_axis',(0.,0.,-1.));
#5952=DIRECTION('center_axis',(1.,0.,0.));
#5953=DIRECTION('ref_axis',(0.,0.,-1.));
#5954=DIRECTION('center_axis',(1.,0.,0.));
#5955=DIRECTION('ref_axis',(0.,0.,-1.));
#5956=DIRECTION('center_axis',(1.,0.,0.));
#5957=DIRECTION('ref_axis',(0.,0.,-1.));
#5958=DIRECTION('center_axis',(-1.,0.,0.));
#5959=DIRECTION('ref_axis',(0.,0.,-1.));
#5960=DIRECTION('center_axis',(1.,0.,0.));
#5961=DIRECTION('ref_axis',(0.,-1.22464679914735E-16,1.));
#5962=DIRECTION('center_axis',(1.,0.,0.));
#5963=DIRECTION('ref_axis',(0.,0.,-1.));
#5964=DIRECTION('center_axis',(1.,0.,0.));
#5965=DIRECTION('ref_axis',(0.,0.,-1.));
#5966=DIRECTION('center_axis',(1.,0.,0.));
#5967=DIRECTION('ref_axis',(0.,0.,-1.));
#5968=DIRECTION('center_axis',(1.,0.,0.));
#5969=DIRECTION('ref_axis',(0.,0.,-1.));
#5970=DIRECTION('center_axis',(1.,0.,0.));
#5971=DIRECTION('ref_axis',(0.,0.,-1.));
#5972=DIRECTION('center_axis',(1.,0.,0.));
#5973=DIRECTION('ref_axis',(0.,0.,-1.));
#5974=DIRECTION('center_axis',(1.,0.,0.));
#5975=DIRECTION('ref_axis',(0.,0.,-1.));
#5976=DIRECTION('center_axis',(1.,0.,0.));
#5977=DIRECTION('ref_axis',(0.,0.,-1.));
#5978=DIRECTION('center_axis',(-1.,0.,0.));
#5979=DIRECTION('ref_axis',(0.,0.,-1.));
#5980=DIRECTION('',(-1.,0.,0.));
#5981=DIRECTION('center_axis',(1.,0.,0.));
#5982=DIRECTION('ref_axis',(0.,0.,-1.));
#5983=DIRECTION('axis',(0.,0.,1.));
#5984=DIRECTION('refdir',(1.,0.,0.));
#5985=DIRECTION('center_axis',(0.0370000185832032,-0.000134528644531496,
0.999315255826152));
#5986=DIRECTION('ref_axis',(-0.999308650506119,0.00363339380273223,0.0370002631492478));
#5987=DIRECTION('center_axis',(0.0370000189191082,0.000134528641494255,
0.999315255813715));
#5988=DIRECTION('ref_axis',(0.351666218592536,-0.936036645094244,-0.0128945624795743));
#5989=DIRECTION('center_axis',(0.0370000189191082,0.000134528641494255,
0.999315255813715));
#5990=DIRECTION('ref_axis',(0.351666218592536,-0.936036645094244,-0.0128945624795743));
#5991=DIRECTION('center_axis',(0.0370000185832032,-0.000134528644531496,
0.999315255826152));
#5992=DIRECTION('ref_axis',(-0.999308650506119,0.00363339380273222,0.0370002631492478));
#5993=DIRECTION('axis',(0.,0.,1.));
#5994=DIRECTION('refdir',(1.,0.,0.));
#5995=DIRECTION('center_axis',(1.,0.,0.));
#5996=DIRECTION('ref_axis',(0.,0.,-1.));
#5997=DIRECTION('',(1.,0.,0.));
#5998=DIRECTION('center_axis',(0.,0.,1.));
#5999=DIRECTION('ref_axis',(1.,0.,0.));
#6000=DIRECTION('center_axis',(0.,0.,1.));
#6001=DIRECTION('ref_axis',(1.,0.,0.));
#6002=DIRECTION('',(0.,0.,1.));
#6003=DIRECTION('center_axis',(0.,0.,-1.));
#6004=DIRECTION('ref_axis',(1.,0.,0.));
#6005=DIRECTION('center_axis',(0.,0.,1.));
#6006=DIRECTION('ref_axis',(1.,0.,0.));
#6007=DIRECTION('center_axis',(0.,0.,1.));
#6008=DIRECTION('ref_axis',(1.,0.,0.));
#6009=DIRECTION('center_axis',(0.,0.,1.));
#6010=DIRECTION('ref_axis',(1.,0.,0.));
#6011=DIRECTION('',(0.,0.,1.));
#6012=DIRECTION('center_axis',(0.,0.,-1.));
#6013=DIRECTION('ref_axis',(1.,0.,0.));
#6014=DIRECTION('center_axis',(0.,0.,1.));
#6015=DIRECTION('ref_axis',(1.,0.,0.));
#6016=DIRECTION('center_axis',(0.,0.,1.));
#6017=DIRECTION('ref_axis',(1.,0.,0.));
#6018=DIRECTION('center_axis',(0.,0.,1.));
#6019=DIRECTION('ref_axis',(1.,0.,0.));
#6020=DIRECTION('',(0.,0.,1.));
#6021=DIRECTION('center_axis',(0.,0.,-1.));
#6022=DIRECTION('ref_axis',(1.,0.,0.));
#6023=DIRECTION('center_axis',(0.,0.,1.));
#6024=DIRECTION('ref_axis',(1.,0.,0.));
#6025=DIRECTION('center_axis',(0.,0.,1.));
#6026=DIRECTION('ref_axis',(1.,0.,0.));
#6027=DIRECTION('center_axis',(0.,0.,1.));
#6028=DIRECTION('ref_axis',(1.,0.,0.));
#6029=DIRECTION('',(0.,0.,1.));
#6030=DIRECTION('center_axis',(0.,0.,-1.));
#6031=DIRECTION('ref_axis',(1.,0.,0.));
#6032=DIRECTION('center_axis',(0.,0.,1.));
#6033=DIRECTION('ref_axis',(1.,0.,0.));
#6034=DIRECTION('center_axis',(0.,0.,1.));
#6035=DIRECTION('ref_axis',(1.,0.,0.));
#6036=DIRECTION('center_axis',(0.,0.,1.));
#6037=DIRECTION('ref_axis',(1.,0.,0.));
#6038=DIRECTION('center_axis',(0.,0.,1.));
#6039=DIRECTION('ref_axis',(1.,0.,0.));
#6040=DIRECTION('center_axis',(0.,0.,1.));
#6041=DIRECTION('ref_axis',(1.,0.,0.));
#6042=DIRECTION('',(0.,0.,1.));
#6043=DIRECTION('center_axis',(0.,0.,1.));
#6044=DIRECTION('ref_axis',(1.,0.,0.));
#6045=DIRECTION('',(0.,0.,-1.));
#6046=DIRECTION('center_axis',(0.,0.,1.));
#6047=DIRECTION('ref_axis',(1.,0.,0.));
#6048=DIRECTION('',(0.,0.,-1.));
#6049=DIRECTION('center_axis',(0.,0.,1.));
#6050=DIRECTION('ref_axis',(1.,0.,0.));
#6051=DIRECTION('',(0.,0.,1.));
#6052=DIRECTION('center_axis',(0.,0.,1.));
#6053=DIRECTION('ref_axis',(1.,0.,0.));
#6054=DIRECTION('center_axis',(0.,0.,1.));
#6055=DIRECTION('ref_axis',(1.,0.,0.));
#6056=DIRECTION('center_axis',(0.,0.,1.));
#6057=DIRECTION('ref_axis',(1.,0.,0.));
#6058=DIRECTION('center_axis',(0.,0.,1.));
#6059=DIRECTION('ref_axis',(-0.707106781186548,-0.707106781186547,0.));
#6060=DIRECTION('',(0.,0.,-1.));
#6061=DIRECTION('center_axis',(0.,0.,1.));
#6062=DIRECTION('ref_axis',(1.,0.,0.));
#6063=DIRECTION('',(0.,0.,1.));
#6064=DIRECTION('center_axis',(0.,0.,1.));
#6065=DIRECTION('ref_axis',(1.,0.,0.));
#6066=DIRECTION('center_axis',(0.,0.,1.));
#6067=DIRECTION('ref_axis',(1.,0.,0.));
#6068=DIRECTION('center_axis',(0.,0.,1.));
#6069=DIRECTION('ref_axis',(1.,0.,0.));
#6070=DIRECTION('center_axis',(0.,0.,1.));
#6071=DIRECTION('ref_axis',(-0.707106781186547,0.707106781186548,0.));
#6072=DIRECTION('',(0.,0.,-1.));
#6073=DIRECTION('center_axis',(0.,0.,1.));
#6074=DIRECTION('ref_axis',(1.,0.,0.));
#6075=DIRECTION('',(0.,0.,1.));
#6076=DIRECTION('center_axis',(0.,0.,1.));
#6077=DIRECTION('ref_axis',(1.,0.,0.));
#6078=DIRECTION('center_axis',(0.,0.,1.));
#6079=DIRECTION('ref_axis',(1.,0.,0.));
#6080=DIRECTION('center_axis',(0.,0.,1.));
#6081=DIRECTION('ref_axis',(1.,0.,0.));
#6082=DIRECTION('center_axis',(0.,0.,1.));
#6083=DIRECTION('ref_axis',(1.,0.,0.));
#6084=DIRECTION('center_axis',(0.,0.,1.));
#6085=DIRECTION('ref_axis',(1.,0.,0.));
#6086=DIRECTION('',(0.,0.,-1.));
#6087=DIRECTION('center_axis',(0.,0.,1.));
#6088=DIRECTION('ref_axis',(1.,0.,0.));
#6089=DIRECTION('center_axis',(0.,0.,1.));
#6090=DIRECTION('ref_axis',(1.,0.,0.));
#6091=DIRECTION('center_axis',(0.,0.,1.));
#6092=DIRECTION('ref_axis',(1.,0.,0.));
#6093=DIRECTION('center_axis',(0.,0.,1.));
#6094=DIRECTION('ref_axis',(1.,0.,0.));
#6095=DIRECTION('center_axis',(0.,0.,1.));
#6096=DIRECTION('ref_axis',(1.,0.,0.));
#6097=DIRECTION('center_axis',(0.,0.,1.));
#6098=DIRECTION('ref_axis',(1.,0.,0.));
#6099=DIRECTION('center_axis',(0.,0.,1.));
#6100=DIRECTION('ref_axis',(1.,0.,0.));
#6101=DIRECTION('center_axis',(0.,0.,-1.));
#6102=DIRECTION('ref_axis',(1.,0.,0.));
#6103=DIRECTION('center_axis',(0.,0.,-1.));
#6104=DIRECTION('ref_axis',(1.,0.,0.));
#6105=DIRECTION('center_axis',(0.,0.,-1.));
#6106=DIRECTION('ref_axis',(1.,0.,0.));
#6107=DIRECTION('center_axis',(0.,0.,-1.));
#6108=DIRECTION('ref_axis',(1.,0.,0.));
#6109=DIRECTION('center_axis',(0.,0.,1.));
#6110=DIRECTION('ref_axis',(1.,0.,0.));
#6111=DIRECTION('center_axis',(0.,0.,1.));
#6112=DIRECTION('ref_axis',(1.,0.,0.));
#6113=DIRECTION('',(0.,0.,1.));
#6114=DIRECTION('center_axis',(0.,0.,1.));
#6115=DIRECTION('ref_axis',(1.,0.,0.));
#6116=DIRECTION('center_axis',(0.,0.,1.));
#6117=DIRECTION('ref_axis',(1.,0.,0.));
#6118=DIRECTION('',(0.,0.,1.));
#6119=DIRECTION('center_axis',(0.,0.,1.));
#6120=DIRECTION('ref_axis',(1.,0.,0.));
#6121=DIRECTION('center_axis',(0.,0.,1.));
#6122=DIRECTION('ref_axis',(1.,0.,0.));
#6123=DIRECTION('',(0.,0.,1.));
#6124=DIRECTION('center_axis',(0.,0.,1.));
#6125=DIRECTION('ref_axis',(1.,0.,0.));
#6126=DIRECTION('center_axis',(0.,0.,1.));
#6127=DIRECTION('ref_axis',(1.,0.,0.));
#6128=DIRECTION('',(0.,0.,1.));
#6129=DIRECTION('center_axis',(0.,0.,1.));
#6130=DIRECTION('ref_axis',(1.,0.,0.));
#6131=DIRECTION('center_axis',(0.,0.,1.));
#6132=DIRECTION('ref_axis',(1.,0.,0.));
#6133=DIRECTION('',(0.,0.,1.));
#6134=DIRECTION('center_axis',(0.,0.,-1.));
#6135=DIRECTION('ref_axis',(1.,0.,0.));
#6136=DIRECTION('center_axis',(0.,0.,1.));
#6137=DIRECTION('ref_axis',(1.,0.,0.));
#6138=DIRECTION('center_axis',(0.,0.,1.));
#6139=DIRECTION('ref_axis',(1.,0.,0.));
#6140=DIRECTION('center_axis',(0.,0.,1.));
#6141=DIRECTION('ref_axis',(1.,0.,0.));
#6142=DIRECTION('',(0.,0.,-1.));
#6143=DIRECTION('center_axis',(0.,0.,1.));
#6144=DIRECTION('ref_axis',(1.,0.,0.));
#6145=DIRECTION('center_axis',(0.,0.,1.));
#6146=DIRECTION('ref_axis',(1.,0.,0.));
#6147=DIRECTION('',(0.,0.,-1.));
#6148=DIRECTION('center_axis',(0.,0.,-1.));
#6149=DIRECTION('ref_axis',(1.,0.,0.));
#6150=DIRECTION('center_axis',(0.,0.,1.));
#6151=DIRECTION('ref_axis',(1.,0.,0.));
#6152=DIRECTION('center_axis',(0.,0.,1.));
#6153=DIRECTION('ref_axis',(1.,0.,0.));
#6154=DIRECTION('axis',(0.,0.,1.));
#6155=DIRECTION('refdir',(1.,0.,0.));
#6156=DIRECTION('center_axis',(0.,0.,1.));
#6157=DIRECTION('ref_axis',(1.,0.,0.));
#6158=DIRECTION('center_axis',(0.,0.,1.));
#6159=DIRECTION('ref_axis',(1.,0.,0.));
#6160=DIRECTION('',(0.,0.,1.));
#6161=DIRECTION('center_axis',(0.,0.,-1.));
#6162=DIRECTION('ref_axis',(1.,0.,0.));
#6163=DIRECTION('center_axis',(0.,0.,1.));
#6164=DIRECTION('ref_axis',(1.,0.,0.));
#6165=DIRECTION('center_axis',(0.,0.,1.));
#6166=DIRECTION('ref_axis',(1.,0.,0.));
#6167=DIRECTION('center_axis',(0.,0.,1.));
#6168=DIRECTION('ref_axis',(1.,0.,0.));
#6169=DIRECTION('center_axis',(0.,0.,1.));
#6170=DIRECTION('ref_axis',(1.,0.,0.));
#6171=DIRECTION('',(0.,0.,1.));
#6172=DIRECTION('center_axis',(0.,0.,-1.));
#6173=DIRECTION('ref_axis',(1.,0.,0.));
#6174=DIRECTION('center_axis',(0.,0.,1.));
#6175=DIRECTION('ref_axis',(1.,0.,0.));
#6176=DIRECTION('center_axis',(0.,0.,1.));
#6177=DIRECTION('ref_axis',(1.,0.,0.));
#6178=DIRECTION('center_axis',(0.,0.,1.));
#6179=DIRECTION('ref_axis',(1.,0.,0.));
#6180=DIRECTION('center_axis',(0.,0.,1.));
#6181=DIRECTION('ref_axis',(1.,0.,0.));
#6182=DIRECTION('',(0.,0.,1.));
#6183=DIRECTION('center_axis',(0.,0.,-1.));
#6184=DIRECTION('ref_axis',(1.,0.,0.));
#6185=DIRECTION('center_axis',(0.,0.,1.));
#6186=DIRECTION('ref_axis',(1.,0.,0.));
#6187=DIRECTION('center_axis',(0.,0.,1.));
#6188=DIRECTION('ref_axis',(1.,0.,0.));
#6189=DIRECTION('center_axis',(0.,0.,1.));
#6190=DIRECTION('ref_axis',(1.,0.,0.));
#6191=DIRECTION('center_axis',(0.,0.,1.));
#6192=DIRECTION('ref_axis',(1.,0.,0.));
#6193=DIRECTION('',(0.,0.,1.));
#6194=DIRECTION('center_axis',(0.,0.,-1.));
#6195=DIRECTION('ref_axis',(1.,0.,0.));
#6196=DIRECTION('center_axis',(0.,0.,1.));
#6197=DIRECTION('ref_axis',(1.,0.,0.));
#6198=DIRECTION('center_axis',(0.,0.,1.));
#6199=DIRECTION('ref_axis',(1.,0.,0.));
#6200=DIRECTION('center_axis',(0.,0.,1.));
#6201=DIRECTION('ref_axis',(1.,0.,0.));
#6202=DIRECTION('center_axis',(0.,0.,1.));
#6203=DIRECTION('ref_axis',(1.,0.,0.));
#6204=DIRECTION('',(0.,0.,1.));
#6205=DIRECTION('center_axis',(0.,0.,1.));
#6206=DIRECTION('ref_axis',(1.,0.,0.));
#6207=DIRECTION('center_axis',(0.,0.,1.));
#6208=DIRECTION('ref_axis',(1.,0.,0.));
#6209=DIRECTION('',(0.,0.,1.));
#6210=DIRECTION('center_axis',(0.,0.,1.));
#6211=DIRECTION('ref_axis',(1.,0.,0.));
#6212=DIRECTION('center_axis',(0.,0.,1.));
#6213=DIRECTION('ref_axis',(1.,0.,0.));
#6214=DIRECTION('',(0.,0.,1.));
#6215=DIRECTION('center_axis',(0.,0.,1.));
#6216=DIRECTION('ref_axis',(1.,0.,0.));
#6217=DIRECTION('center_axis',(0.,0.,1.));
#6218=DIRECTION('ref_axis',(1.,0.,0.));
#6219=DIRECTION('',(0.,0.,1.));
#6220=DIRECTION('center_axis',(0.,0.,1.));
#6221=DIRECTION('ref_axis',(1.,0.,0.));
#6222=DIRECTION('center_axis',(0.,0.,1.));
#6223=DIRECTION('ref_axis',(1.,0.,0.));
#6224=DIRECTION('',(0.,0.,-1.));
#6225=DIRECTION('center_axis',(0.,0.,1.));
#6226=DIRECTION('ref_axis',(1.,0.,0.));
#6227=DIRECTION('center_axis',(0.,0.,1.));
#6228=DIRECTION('ref_axis',(1.,0.,0.));
#6229=DIRECTION('center_axis',(0.,0.,-1.));
#6230=DIRECTION('ref_axis',(1.,0.,0.));
#6231=DIRECTION('center_axis',(0.,0.,1.));
#6232=DIRECTION('ref_axis',(1.,0.,0.));
#6233=DIRECTION('center_axis',(0.,0.,-1.));
#6234=DIRECTION('ref_axis',(1.,0.,0.));
#6235=DIRECTION('',(0.,0.,-1.));
#6236=DIRECTION('center_axis',(0.,0.,1.));
#6237=DIRECTION('ref_axis',(1.,0.,0.));
#6238=DIRECTION('center_axis',(0.,0.,1.));
#6239=DIRECTION('ref_axis',(1.,0.,0.));
#6240=DIRECTION('',(0.,0.,-1.));
#6241=DIRECTION('center_axis',(0.,0.,1.));
#6242=DIRECTION('ref_axis',(1.,0.,0.));
#6243=DIRECTION('center_axis',(0.,0.,1.));
#6244=DIRECTION('ref_axis',(1.,0.,0.));
#6245=DIRECTION('center_axis',(0.,0.,1.));
#6246=DIRECTION('ref_axis',(1.,0.,0.));
#6247=DIRECTION('axis',(0.,0.,1.));
#6248=DIRECTION('refdir',(1.,0.,0.));
#6249=DIRECTION('axis',(0.,0.,1.));
#6250=DIRECTION('refdir',(1.,0.,0.));
#6251=DIRECTION('center_axis',(0.,1.,0.));
#6252=DIRECTION('ref_axis',(0.,0.,1.));
#6253=DIRECTION('center_axis',(0.,-1.,0.));
#6254=DIRECTION('ref_axis',(1.,0.,0.));
#6255=DIRECTION('',(-1.,0.,0.));
#6256=DIRECTION('',(0.,0.,-1.));
#6257=DIRECTION('',(1.,0.,0.));
#6258=DIRECTION('center_axis',(0.,0.,1.));
#6259=DIRECTION('ref_axis',(1.,0.,0.));
#6260=DIRECTION('',(0.,-1.,0.));
#6261=DIRECTION('',(0.,1.,0.));
#6262=DIRECTION('',(-1.,0.,0.));
#6263=DIRECTION('center_axis',(0.,-1.,0.));
#6264=DIRECTION('ref_axis',(0.,0.,-1.));
#6265=DIRECTION('center_axis',(0.,1.,0.));
#6266=DIRECTION('ref_axis',(1.,0.,0.));
#6267=DIRECTION('',(0.,0.,1.));
#6268=DIRECTION('',(1.,0.,0.));
#6269=DIRECTION('center_axis',(0.,0.,-1.));
#6270=DIRECTION('ref_axis',(-1.,0.,0.));
#6271=DIRECTION('',(0.,1.,0.));
#6272=DIRECTION('',(0.,1.,0.));
#6273=DIRECTION('center_axis',(1.,0.,0.));
#6274=DIRECTION('ref_axis',(0.,0.,-1.));
#6275=DIRECTION('center_axis',(0.,1.,0.));
#6276=DIRECTION('ref_axis',(0.,0.,1.));
#6277=DIRECTION('center_axis',(0.,-1.,0.));
#6278=DIRECTION('ref_axis',(1.,0.,0.));
#6279=DIRECTION('center_axis',(0.,-1.,0.));
#6280=DIRECTION('ref_axis',(1.,0.,0.));
#6281=DIRECTION('center_axis',(0.,-1.,0.));
#6282=DIRECTION('ref_axis',(1.,0.,0.));
#6283=DIRECTION('center_axis',(0.,-1.,0.));
#6284=DIRECTION('ref_axis',(1.,0.,0.));
#6285=DIRECTION('',(0.,1.,0.));
#6286=DIRECTION('center_axis',(0.,-1.,0.));
#6287=DIRECTION('ref_axis',(0.,0.,-1.));
#6288=DIRECTION('center_axis',(0.,-1.,0.));
#6289=DIRECTION('ref_axis',(1.,0.,0.));
#6290=DIRECTION('center_axis',(0.,-1.,0.));
#6291=DIRECTION('ref_axis',(1.,0.,0.));
#6292=DIRECTION('center_axis',(0.,-1.,0.));
#6293=DIRECTION('ref_axis',(1.,0.,0.));
#6294=DIRECTION('',(0.,1.,0.));
#6295=DIRECTION('center_axis',(0.,1.,0.));
#6296=DIRECTION('ref_axis',(0.,0.,1.));
#6297=DIRECTION('center_axis',(0.,-1.,0.));
#6298=DIRECTION('ref_axis',(1.,0.,0.));
#6299=DIRECTION('center_axis',(0.,-1.,0.));
#6300=DIRECTION('ref_axis',(1.,0.,0.));
#6301=DIRECTION('center_axis',(0.,-1.,0.));
#6302=DIRECTION('ref_axis',(1.,0.,0.));
#6303=DIRECTION('',(0.,1.,0.));
#6304=DIRECTION('center_axis',(0.,-1.,0.));
#6305=DIRECTION('ref_axis',(0.,0.,-1.));
#6306=DIRECTION('center_axis',(0.,-1.,0.));
#6307=DIRECTION('ref_axis',(1.,0.,0.));
#6308=DIRECTION('center_axis',(0.,-1.,0.));
#6309=DIRECTION('ref_axis',(1.,0.,0.));
#6310=DIRECTION('center_axis',(0.,-1.,0.));
#6311=DIRECTION('ref_axis',(1.,0.,0.));
#6312=DIRECTION('',(0.,1.,0.));
#6313=DIRECTION('center_axis',(0.,1.,0.));
#6314=DIRECTION('ref_axis',(0.,0.,1.));
#6315=DIRECTION('center_axis',(0.,-1.,0.));
#6316=DIRECTION('ref_axis',(1.,0.,0.));
#6317=DIRECTION('center_axis',(0.,-1.,0.));
#6318=DIRECTION('ref_axis',(1.,0.,0.));
#6319=DIRECTION('center_axis',(0.,-1.,0.));
#6320=DIRECTION('ref_axis',(1.,0.,0.));
#6321=DIRECTION('',(0.,1.,0.));
#6322=DIRECTION('center_axis',(0.,-1.,0.));
#6323=DIRECTION('ref_axis',(0.,0.,-1.));
#6324=DIRECTION('center_axis',(0.,-1.,0.));
#6325=DIRECTION('ref_axis',(1.,0.,0.));
#6326=DIRECTION('center_axis',(0.,-1.,0.));
#6327=DIRECTION('ref_axis',(1.,0.,0.));
#6328=DIRECTION('',(0.,1.,0.));
#6329=DIRECTION('axis',(0.,0.,1.));
#6330=DIRECTION('refdir',(1.,0.,0.));
#6331=DIRECTION('center_axis',(0.,1.,0.));
#6332=DIRECTION('ref_axis',(0.,0.,1.));
#6333=DIRECTION('center_axis',(0.,1.,0.));
#6334=DIRECTION('ref_axis',(1.,0.,0.));
#6335=DIRECTION('',(1.,0.,0.));
#6336=DIRECTION('center_axis',(0.,-1.,0.));
#6337=DIRECTION('ref_axis',(1.,0.,0.));
#6338=DIRECTION('',(-1.,0.,0.));
#6339=DIRECTION('center_axis',(0.,0.,-1.));
#6340=DIRECTION('ref_axis',(-1.,0.,0.));
#6341=DIRECTION('',(0.,-1.,0.));
#6342=DIRECTION('',(0.,1.,0.));
#6343=DIRECTION('',(1.,0.,0.));
#6344=DIRECTION('center_axis',(0.,-1.,0.));
#6345=DIRECTION('ref_axis',(0.,0.,-1.));
#6346=DIRECTION('center_axis',(0.,-1.,0.));
#6347=DIRECTION('ref_axis',(1.,0.,0.));
#6348=DIRECTION('center_axis',(0.,1.,0.));
#6349=DIRECTION('ref_axis',(1.,0.,0.));
#6350=DIRECTION('',(-1.,0.,0.));
#6351=DIRECTION('center_axis',(0.,0.,1.));
#6352=DIRECTION('ref_axis',(1.,0.,0.));
#6353=DIRECTION('',(0.,1.,0.));
#6354=DIRECTION('',(0.,-1.,0.));
#6355=DIRECTION('center_axis',(0.,1.,0.));
#6356=DIRECTION('ref_axis',(0.,0.,1.));
#6357=DIRECTION('center_axis',(0.,-1.,0.));
#6358=DIRECTION('ref_axis',(1.,0.,0.));
#6359=DIRECTION('center_axis',(0.,-1.,0.));
#6360=DIRECTION('ref_axis',(1.,0.,0.));
#6361=DIRECTION('center_axis',(0.,-1.,0.));
#6362=DIRECTION('ref_axis',(1.,0.,0.));
#6363=DIRECTION('center_axis',(0.,-1.,0.));
#6364=DIRECTION('ref_axis',(1.,0.,0.));
#6365=DIRECTION('',(0.,1.,0.));
#6366=DIRECTION('center_axis',(0.,-1.,0.));
#6367=DIRECTION('ref_axis',(0.,0.,-1.));
#6368=DIRECTION('center_axis',(0.,-1.,0.));
#6369=DIRECTION('ref_axis',(1.,0.,0.));
#6370=DIRECTION('center_axis',(0.,-1.,0.));
#6371=DIRECTION('ref_axis',(1.,0.,0.));
#6372=DIRECTION('',(0.,1.,0.));
#6373=DIRECTION('',(0.,0.,1.));
#6374=DIRECTION('',(1.,0.,0.));
#6375=DIRECTION('',(0.,0.,1.));
#6376=DIRECTION('',(1.,0.,0.));
#6377=DIRECTION('axis',(0.,0.,1.));
#6378=DIRECTION('refdir',(1.,0.,0.));
#6379=DIRECTION('center_axis',(0.866025403784439,0.,-0.5));
#6380=DIRECTION('ref_axis',(0.5,0.,0.866025403784439));
#6381=DIRECTION('',(-0.5,0.,-0.866025403784439));
#6382=DIRECTION('',(0.,-1.,0.));
#6383=DIRECTION('',(0.5,0.,0.866025403784439));
#6384=DIRECTION('',(0.,-1.,0.));
#6385=DIRECTION('center_axis',(1.20185167898973E-16,0.,-1.));
#6386=DIRECTION('ref_axis',(1.,0.,1.20185167898973E-16));
#6387=DIRECTION('',(-1.,0.,-1.20185167898973E-16));
#6388=DIRECTION('',(0.,-1.,0.));
#6389=DIRECTION('',(1.,0.,1.20185167898973E-16));
#6390=DIRECTION('center_axis',(-0.866025403784439,0.,-0.5));
#6391=DIRECTION('ref_axis',(0.5,0.,-0.866025403784439));
#6392=DIRECTION('',(-0.5,0.,0.866025403784439));
#6393=DIRECTION('',(0.,-1.,0.));
#6394=DIRECTION('',(0.5,0.,-0.866025403784439));
#6395=DIRECTION('center_axis',(-0.866025403784439,0.,0.5));
#6396=DIRECTION('ref_axis',(-0.5,0.,-0.866025403784439));
#6397=DIRECTION('',(0.5,0.,0.866025403784439));
#6398=DIRECTION('',(0.,-1.,0.));
#6399=DIRECTION('',(-0.5,0.,-0.866025403784439));
#6400=DIRECTION('center_axis',(-2.40370335797945E-16,0.,1.));
#6401=DIRECTION('ref_axis',(-1.,0.,-2.40370335797945E-16));
#6402=DIRECTION('',(1.,0.,2.40370335797945E-16));
#6403=DIRECTION('',(0.,-1.,0.));
#6404=DIRECTION('',(-1.,0.,-2.40370335797945E-16));
#6405=DIRECTION('center_axis',(0.866025403784439,0.,0.5));
#6406=DIRECTION('ref_axis',(-0.5,0.,0.866025403784439));
#6407=DIRECTION('',(0.5,0.,-0.866025403784439));
#6408=DIRECTION('',(-0.5,0.,0.866025403784439));
#6409=DIRECTION('center_axis',(0.,1.,0.));
#6410=DIRECTION('ref_axis',(1.,0.,0.));
#6411=DIRECTION('center_axis',(0.,-1.,0.));
#6412=DIRECTION('ref_axis',(0.,0.,-1.));
#6413=DIRECTION('center_axis',(0.,1.,0.));
#6414=DIRECTION('ref_axis',(1.,0.,0.));
#6415=DIRECTION('center_axis',(0.,1.,0.));
#6416=DIRECTION('ref_axis',(1.,0.,0.));
#6417=DIRECTION('center_axis',(0.,1.,0.));
#6418=DIRECTION('ref_axis',(0.,0.,1.));
#6419=DIRECTION('center_axis',(0.,-1.,0.));
#6420=DIRECTION('ref_axis',(1.,0.,0.));
#6421=DIRECTION('center_axis',(0.,-1.,0.));
#6422=DIRECTION('ref_axis',(1.,0.,0.));
#6423=DIRECTION('center_axis',(0.,-1.,0.));
#6424=DIRECTION('ref_axis',(1.,0.,0.));
#6425=DIRECTION('',(0.707106781186548,0.707106781186547,8.65956056235493E-17));
#6426=DIRECTION('center_axis',(0.,-1.,0.));
#6427=DIRECTION('ref_axis',(1.,0.,0.));
#6428=DIRECTION('center_axis',(0.,-1.,0.));
#6429=DIRECTION('ref_axis',(1.,0.,0.));
#6430=DIRECTION('',(0.,1.,0.));
#6431=DIRECTION('center_axis',(0.,1.,0.));
#6432=DIRECTION('ref_axis',(1.,0.,0.));
#6433=DIRECTION('center_axis',(0.,-1.,0.));
#6434=DIRECTION('ref_axis',(1.,0.,0.));
#6435=DIRECTION('',(-0.707106781186547,0.707106781186548,-8.65956056235493E-17));
#6436=DIRECTION('center_axis',(0.,-1.,0.));
#6437=DIRECTION('ref_axis',(0.,0.,-1.));
#6438=DIRECTION('center_axis',(0.,-1.,0.));
#6439=DIRECTION('ref_axis',(1.,0.,0.));
#6440=DIRECTION('center_axis',(0.,1.,0.));
#6441=DIRECTION('ref_axis',(1.,0.,0.));
#6442=DIRECTION('center_axis',(0.,1.,0.));
#6443=DIRECTION('ref_axis',(1.,0.,0.));
#6444=DIRECTION('',(-0.447213595499958,0.894427190999916,-5.47678698264203E-17));
#6445=DIRECTION('center_axis',(0.,-1.,0.));
#6446=DIRECTION('ref_axis',(1.,0.,0.));
#6447=DIRECTION('',(0.,1.,0.));
#6448=DIRECTION('axis',(0.,0.,1.));
#6449=DIRECTION('refdir',(1.,0.,0.));
#6450=DIRECTION('axis',(0.,0.,1.));
#6451=DIRECTION('refdir',(1.,0.,0.));
#6452=DIRECTION('center_axis',(0.,0.,1.));
#6453=DIRECTION('ref_axis',(1.,0.,0.));
#6454=DIRECTION('center_axis',(0.,0.,1.));
#6455=DIRECTION('ref_axis',(1.,0.,0.));
#6456=DIRECTION('center_axis',(0.,0.,1.));
#6457=DIRECTION('ref_axis',(1.,0.,0.));
#6458=DIRECTION('center_axis',(0.,0.,1.));
#6459=DIRECTION('ref_axis',(1.,0.,0.));
#6460=DIRECTION('center_axis',(0.,0.,1.));
#6461=DIRECTION('ref_axis',(1.,0.,0.));
#6462=DIRECTION('center_axis',(0.,0.,1.));
#6463=DIRECTION('ref_axis',(1.,0.,0.));
#6464=DIRECTION('center_axis',(0.,0.,1.));
#6465=DIRECTION('ref_axis',(1.,0.,0.));
#6466=DIRECTION('',(0.,0.,-1.));
#6467=DIRECTION('center_axis',(0.,0.,1.));
#6468=DIRECTION('ref_axis',(1.,0.,0.));
#6469=DIRECTION('center_axis',(0.,0.,1.));
#6470=DIRECTION('ref_axis',(1.,0.,0.));
#6471=DIRECTION('center_axis',(0.,0.,-1.));
#6472=DIRECTION('ref_axis',(1.,0.,0.));
#6473=DIRECTION('center_axis',(0.,0.,1.));
#6474=DIRECTION('ref_axis',(1.,0.,0.));
#6475=DIRECTION('',(0.,0.,-1.));
#6476=DIRECTION('center_axis',(0.,0.,1.));
#6477=DIRECTION('ref_axis',(1.,0.,0.));
#6478=DIRECTION('',(0.,0.,-1.));
#6479=DIRECTION('center_axis',(0.,0.,1.));
#6480=DIRECTION('ref_axis',(1.,0.,0.));
#6481=DIRECTION('center_axis',(0.,0.,1.));
#6482=DIRECTION('ref_axis',(1.,0.,0.));
#6483=DIRECTION('center_axis',(0.,0.,1.));
#6484=DIRECTION('ref_axis',(1.,0.,0.));
#6485=DIRECTION('',(0.,0.,-1.));
#6486=DIRECTION('center_axis',(0.,0.,1.));
#6487=DIRECTION('ref_axis',(1.,0.,0.));
#6488=DIRECTION('center_axis',(0.,0.,1.));
#6489=DIRECTION('ref_axis',(1.,0.,0.));
#6490=DIRECTION('axis',(0.,0.,1.));
#6491=DIRECTION('refdir',(1.,0.,0.));
#6492=DIRECTION('center_axis',(0.,0.,1.));
#6493=DIRECTION('ref_axis',(1.,0.,0.));
#6494=DIRECTION('center_axis',(0.,0.,-1.));
#6495=DIRECTION('ref_axis',(1.,0.,0.));
#6496=DIRECTION('',(0.,0.,-1.));
#6497=DIRECTION('center_axis',(0.,0.,-1.));
#6498=DIRECTION('ref_axis',(1.,0.,0.));
#6499=DIRECTION('center_axis',(0.,0.,1.));
#6500=DIRECTION('ref_axis',(1.,0.,0.));
#6501=DIRECTION('center_axis',(0.,0.,1.));
#6502=DIRECTION('ref_axis',(1.,0.,0.));
#6503=DIRECTION('',(0.,0.,-1.));
#6504=DIRECTION('center_axis',(0.,0.,1.));
#6505=DIRECTION('ref_axis',(1.,0.,0.));
#6506=DIRECTION('center_axis',(0.,0.,1.));
#6507=DIRECTION('ref_axis',(1.,0.,0.));
#6508=DIRECTION('center_axis',(0.,0.,1.));
#6509=DIRECTION('ref_axis',(1.,0.,0.));
#6510=DIRECTION('axis',(0.,0.,1.));
#6511=DIRECTION('refdir',(1.,0.,0.));
#6512=DIRECTION('center_axis',(1.,0.,0.));
#6513=DIRECTION('ref_axis',(0.,0.,-1.));
#6514=DIRECTION('',(0.,0.,1.));
#6515=DIRECTION('center_axis',(1.,0.,0.));
#6516=DIRECTION('ref_axis',(0.,0.,-1.));
#6517=DIRECTION('center_axis',(1.,0.,0.));
#6518=DIRECTION('ref_axis',(0.,0.,-1.));
#6519=DIRECTION('center_axis',(1.,0.,0.));
#6520=DIRECTION('ref_axis',(0.,0.,-1.));
#6521=DIRECTION('',(1.,0.,0.));
#6522=DIRECTION('center_axis',(1.,0.,0.));
#6523=DIRECTION('ref_axis',(0.,0.,-1.));
#6524=DIRECTION('',(0.,0.,-1.));
#6525=DIRECTION('center_axis',(0.,0.,1.));
#6526=DIRECTION('ref_axis',(1.,0.,0.));
#6527=DIRECTION('center_axis',(0.,0.,-1.));
#6528=DIRECTION('ref_axis',(1.,0.,0.));
#6529=DIRECTION('',(0.,0.,-1.));
#6530=DIRECTION('center_axis',(0.,0.,-1.));
#6531=DIRECTION('ref_axis',(1.,0.,0.));
#6532=DIRECTION('center_axis',(0.,0.,1.));
#6533=DIRECTION('ref_axis',(1.,0.,0.));
#6534=DIRECTION('center_axis',(0.,0.,1.));
#6535=DIRECTION('ref_axis',(1.,0.,0.));
#6536=DIRECTION('',(0.,0.,-1.));
#6537=DIRECTION('center_axis',(0.,0.,1.));
#6538=DIRECTION('ref_axis',(1.,0.,0.));
#6539=DIRECTION('center_axis',(0.,0.,1.));
#6540=DIRECTION('ref_axis',(1.,0.,0.));
#6541=DIRECTION('center_axis',(0.,0.,1.));
#6542=DIRECTION('ref_axis',(1.,0.,0.));
#6543=DIRECTION('axis',(0.,0.,1.));
#6544=DIRECTION('refdir',(1.,0.,0.));
#6545=DIRECTION('center_axis',(0.,1.,0.));
#6546=DIRECTION('ref_axis',(1.,0.,0.));
#6547=DIRECTION('center_axis',(0.,1.,0.));
#6548=DIRECTION('ref_axis',(1.,0.,0.));
#6549=DIRECTION('center_axis',(0.866025403784439,0.,-0.5));
#6550=DIRECTION('ref_axis',(0.5,0.,0.866025403784439));
#6551=DIRECTION('',(0.5,0.,0.866025403784439));
#6552=DIRECTION('',(0.,-1.,0.));
#6553=DIRECTION('',(0.5,0.,0.866025403784439));
#6554=DIRECTION('',(0.,-1.,0.));
#6555=DIRECTION('center_axis',(1.20185167898973E-16,0.,-1.));
#6556=DIRECTION('ref_axis',(1.,0.,1.20185167898973E-16));
#6557=DIRECTION('',(1.,0.,1.20185167898973E-16));
#6558=DIRECTION('',(0.,-1.,0.));
#6559=DIRECTION('',(1.,0.,1.20185167898973E-16));
#6560=DIRECTION('center_axis',(-0.866025403784439,0.,-0.5));
#6561=DIRECTION('ref_axis',(0.5,0.,-0.866025403784439));
#6562=DIRECTION('',(0.5,0.,-0.866025403784439));
#6563=DIRECTION('',(0.,-1.,0.));
#6564=DIRECTION('',(0.5,0.,-0.866025403784439));
#6565=DIRECTION('center_axis',(-0.866025403784439,0.,0.5));
#6566=DIRECTION('ref_axis',(-0.5,0.,-0.866025403784439));
#6567=DIRECTION('',(-0.5,0.,-0.866025403784439));
#6568=DIRECTION('',(0.,-1.,0.));
#6569=DIRECTION('',(-0.5,0.,-0.866025403784439));
#6570=DIRECTION('center_axis',(-2.40370335797945E-16,0.,1.));
#6571=DIRECTION('ref_axis',(-1.,0.,-2.40370335797945E-16));
#6572=DIRECTION('',(-1.,0.,-2.40370335797945E-16));
#6573=DIRECTION('',(0.,-1.,0.));
#6574=DIRECTION('',(-1.,0.,-2.40370335797945E-16));
#6575=DIRECTION('center_axis',(0.866025403784439,0.,0.5));
#6576=DIRECTION('ref_axis',(-0.5,0.,0.866025403784439));
#6577=DIRECTION('',(-0.5,0.,0.866025403784439));
#6578=DIRECTION('',(-0.5,0.,0.866025403784439));
#6579=DIRECTION('center_axis',(0.,-1.,0.));
#6580=DIRECTION('ref_axis',(0.,0.,-1.));
#6581=DIRECTION('center_axis',(0.,1.,0.));
#6582=DIRECTION('ref_axis',(0.,0.,1.));
#6583=DIRECTION('center_axis',(0.,-1.,0.));
#6584=DIRECTION('ref_axis',(1.,0.,0.));
#6585=DIRECTION('center_axis',(0.,-1.,0.));
#6586=DIRECTION('ref_axis',(1.,0.,0.));
#6587=DIRECTION('center_axis',(0.,-1.,0.));
#6588=DIRECTION('ref_axis',(1.,0.,0.));
#6589=DIRECTION('',(0.707106781186548,0.707106781186547,8.65956056235494E-17));
#6590=DIRECTION('center_axis',(0.,-1.,0.));
#6591=DIRECTION('ref_axis',(1.,0.,0.));
#6592=DIRECTION('',(0.,1.,0.));
#6593=DIRECTION('',(0.,0.,1.));
#6594=DIRECTION('',(1.,0.,0.));
#6595=DIRECTION('',(0.,0.,1.));
#6596=DIRECTION('',(1.,0.,0.));
#6597=DIRECTION('',(0.,0.,1.));
#6598=DIRECTION('',(1.,0.,0.));
#6599=DIRECTION('',(0.,0.,1.));
#6600=DIRECTION('',(2.22044604925031E-16,-1.,0.));
#6601=DIRECTION('axis',(0.,0.,1.));
#6602=DIRECTION('refdir',(1.,0.,0.));
#6603=DIRECTION('axis',(0.,0.,1.));
#6604=DIRECTION('refdir',(1.,0.,0.));
#6605=DIRECTION('center_axis',(1.,0.,0.));
#6606=DIRECTION('ref_axis',(0.,0.,-1.));
#6607=DIRECTION('',(0.,0.,1.));
#6608=DIRECTION('center_axis',(1.,0.,0.));
#6609=DIRECTION('ref_axis',(0.,0.,-1.));
#6610=DIRECTION('center_axis',(1.,0.,0.));
#6611=DIRECTION('ref_axis',(0.,0.,-1.));
#6612=DIRECTION('',(0.,0.,-1.));
#6613=DIRECTION('center_axis',(1.,0.,0.));
#6614=DIRECTION('ref_axis',(0.,0.,-1.));
#6615=DIRECTION('center_axis',(1.,0.,0.));
#6616=DIRECTION('ref_axis',(0.,0.,-1.));
#6617=DIRECTION('',(-1.,0.,0.));
#6618=DIRECTION('center_axis',(1.,0.,0.));
#6619=DIRECTION('ref_axis',(0.,0.,-1.));
#6620=DIRECTION('',(1.,0.,0.));
#6621=DIRECTION('center_axis',(1.,0.,0.));
#6622=DIRECTION('ref_axis',(0.,0.,-1.));
#6623=DIRECTION('',(1.,0.,0.));
#6624=DIRECTION('',(-1.,0.,0.));
#6625=DIRECTION('center_axis',(1.,0.,0.));
#6626=DIRECTION('ref_axis',(0.,0.,-1.));
#6627=DIRECTION('center_axis',(1.,0.,0.));
#6628=DIRECTION('ref_axis',(0.,0.,-1.));
#6629=DIRECTION('',(0.,0.,1.));
#6630=DIRECTION('',(0.,-1.,0.));
#6631=DIRECTION('',(0.,0.,-1.));
#6632=DIRECTION('',(0.,0.,-1.));
#6633=DIRECTION('',(0.,1.,0.));
#6634=DIRECTION('',(0.,0.,1.));
#6635=DIRECTION('center_axis',(1.,0.,0.));
#6636=DIRECTION('ref_axis',(0.,0.,-1.));
#6637=DIRECTION('center_axis',(0.,-1.,0.));
#6638=DIRECTION('ref_axis',(0.,0.,-1.));
#6639=DIRECTION('',(1.,0.,0.));
#6640=DIRECTION('',(0.,0.,1.));
#6641=DIRECTION('',(1.,0.,0.));
#6642=DIRECTION('',(0.,0.,-1.));
#6643=DIRECTION('',(1.,0.,0.));
#6644=DIRECTION('',(0.,0.,1.));
#6645=DIRECTION('',(1.,0.,0.));
#6646=DIRECTION('center_axis',(0.,0.,1.));
#6647=DIRECTION('ref_axis',(1.,0.,0.));
#6648=DIRECTION('center_axis',(0.,0.,1.));
#6649=DIRECTION('ref_axis',(1.,0.,0.));
#6650=DIRECTION('',(0.,0.,1.));
#6651=DIRECTION('center_axis',(0.,0.,-1.));
#6652=DIRECTION('ref_axis',(1.,0.,0.));
#6653=DIRECTION('center_axis',(0.,0.,1.));
#6654=DIRECTION('ref_axis',(1.,0.,0.));
#6655=DIRECTION('center_axis',(0.,0.,1.));
#6656=DIRECTION('ref_axis',(1.,0.,0.));
#6657=DIRECTION('',(0.,0.,1.));
#6658=DIRECTION('center_axis',(0.,0.,-1.));
#6659=DIRECTION('ref_axis',(1.,0.,0.));
#6660=DIRECTION('center_axis',(0.,0.,1.));
#6661=DIRECTION('ref_axis',(-1.,1.22464679914735E-16,0.));
#6662=DIRECTION('',(0.,0.,1.));
#6663=DIRECTION('center_axis',(0.,0.,1.));
#6664=DIRECTION('ref_axis',(1.,0.,0.));
#6665=DIRECTION('center_axis',(0.,0.,1.));
#6666=DIRECTION('ref_axis',(1.,0.,0.));
#6667=DIRECTION('center_axis',(0.,0.,1.));
#6668=DIRECTION('ref_axis',(0.,-1.,0.));
#6669=DIRECTION('',(1.,0.,0.));
#6670=DIRECTION('center_axis',(0.,0.,1.));
#6671=DIRECTION('ref_axis',(1.,0.,0.));
#6672=DIRECTION('',(-1.,0.,0.));
#6673=DIRECTION('',(0.,1.,0.));
#6674=DIRECTION('center_axis',(0.,1.,0.));
#6675=DIRECTION('ref_axis',(0.,0.,1.));
#6676=DIRECTION('',(1.,0.,0.));
#6677=DIRECTION('',(0.,0.,1.));
#6678=DIRECTION('',(-1.,0.,0.));
#6679=DIRECTION('',(0.,0.,1.));
#6680=DIRECTION('center_axis',(0.,0.,1.));
#6681=DIRECTION('ref_axis',(-1.,-1.22464679914735E-16,0.));
#6682=DIRECTION('center_axis',(0.,0.,1.));
#6683=DIRECTION('ref_axis',(1.,0.,0.));
#6684=DIRECTION('center_axis',(0.,0.,1.));
#6685=DIRECTION('ref_axis',(1.,0.,0.));
#6686=DIRECTION('center_axis',(0.,0.,-1.));
#6687=DIRECTION('ref_axis',(0.,1.,0.));
#6688=DIRECTION('center_axis',(0.,0.,1.));
#6689=DIRECTION('ref_axis',(1.,0.,0.));
#6690=DIRECTION('',(0.,-1.,0.));
#6691=DIRECTION('center_axis',(1.,0.,0.));
#6692=DIRECTION('ref_axis',(0.,0.,-1.));
#6693=DIRECTION('center_axis',(1.,0.,0.));
#6694=DIRECTION('ref_axis',(0.,0.,-1.));
#6695=DIRECTION('',(-1.,0.,0.));
#6696=DIRECTION('center_axis',(1.,0.,0.));
#6697=DIRECTION('ref_axis',(0.,0.,-1.));
#6698=DIRECTION('center_axis',(1.,0.,0.));
#6699=DIRECTION('ref_axis',(0.,0.,-1.));
#6700=DIRECTION('axis',(0.,0.,1.));
#6701=DIRECTION('refdir',(1.,0.,0.));
#6702=DIRECTION('center_axis',(0.,0.,1.));
#6703=DIRECTION('ref_axis',(1.,0.,0.));
#6704=DIRECTION('center_axis',(0.,0.,1.));
#6705=DIRECTION('ref_axis',(1.,0.,0.));
#6706=DIRECTION('',(0.,0.,1.));
#6707=DIRECTION('center_axis',(0.,0.,-1.));
#6708=DIRECTION('ref_axis',(1.,0.,0.));
#6709=DIRECTION('center_axis',(0.,0.,1.));
#6710=DIRECTION('ref_axis',(1.,0.,0.));
#6711=DIRECTION('center_axis',(0.,0.,1.));
#6712=DIRECTION('ref_axis',(1.,0.,0.));
#6713=DIRECTION('center_axis',(0.,0.,1.));
#6714=DIRECTION('ref_axis',(1.,0.,0.));
#6715=DIRECTION('center_axis',(0.,0.,1.));
#6716=DIRECTION('ref_axis',(1.,0.,0.));
#6717=DIRECTION('center_axis',(0.,0.,1.));
#6718=DIRECTION('ref_axis',(1.,0.,0.));
#6719=DIRECTION('',(0.,0.,-1.));
#6720=DIRECTION('center_axis',(0.,0.,1.));
#6721=DIRECTION('ref_axis',(1.,0.,0.));
#6722=DIRECTION('center_axis',(0.,0.,1.));
#6723=DIRECTION('ref_axis',(1.,0.,0.));
#6724=DIRECTION('center_axis',(0.,0.,1.));
#6725=DIRECTION('ref_axis',(1.,0.,0.));
#6726=DIRECTION('center_axis',(0.,0.,1.));
#6727=DIRECTION('ref_axis',(1.,0.,0.));
#6728=DIRECTION('',(0.,0.,-1.));
#6729=DIRECTION('center_axis',(0.,0.,1.));
#6730=DIRECTION('ref_axis',(1.,0.,0.));
#6731=DIRECTION('axis',(0.,0.,1.));
#6732=DIRECTION('refdir',(1.,0.,0.));
#6733=DIRECTION('center_axis',(0.,0.,1.));
#6734=DIRECTION('ref_axis',(1.,0.,0.));
#6735=DIRECTION('center_axis',(0.,0.,-1.));
#6736=DIRECTION('ref_axis',(1.,0.,0.));
#6737=DIRECTION('',(0.,0.,-1.));
#6738=DIRECTION('center_axis',(0.,0.,-1.));
#6739=DIRECTION('ref_axis',(1.,0.,0.));
#6740=DIRECTION('center_axis',(0.,0.,1.));
#6741=DIRECTION('ref_axis',(1.,0.,0.));
#6742=DIRECTION('center_axis',(0.,0.,1.));
#6743=DIRECTION('ref_axis',(1.,0.,0.));
#6744=DIRECTION('',(0.,0.,-1.));
#6745=DIRECTION('center_axis',(0.,0.,1.));
#6746=DIRECTION('ref_axis',(1.,0.,0.));
#6747=DIRECTION('center_axis',(0.,0.,1.));
#6748=DIRECTION('ref_axis',(1.,0.,0.));
#6749=DIRECTION('center_axis',(0.,0.,1.));
#6750=DIRECTION('ref_axis',(1.,0.,0.));
#6751=DIRECTION('axis',(0.,0.,1.));
#6752=DIRECTION('refdir',(1.,0.,0.));
#6753=DIRECTION('center_axis',(0.,0.,1.));
#6754=DIRECTION('ref_axis',(1.,0.,0.));
#6755=DIRECTION('center_axis',(0.,0.,-1.));
#6756=DIRECTION('ref_axis',(1.,0.,0.));
#6757=DIRECTION('',(0.,0.,-1.));
#6758=DIRECTION('center_axis',(0.,0.,-1.));
#6759=DIRECTION('ref_axis',(1.,0.,0.));
#6760=DIRECTION('center_axis',(0.,0.,1.));
#6761=DIRECTION('ref_axis',(1.,0.,0.));
#6762=DIRECTION('center_axis',(0.,0.,1.));
#6763=DIRECTION('ref_axis',(1.,0.,0.));
#6764=DIRECTION('',(0.,0.,-1.));
#6765=DIRECTION('center_axis',(0.,0.,1.));
#6766=DIRECTION('ref_axis',(1.,0.,0.));
#6767=DIRECTION('center_axis',(0.,0.,1.));
#6768=DIRECTION('ref_axis',(1.,0.,0.));
#6769=DIRECTION('center_axis',(0.,0.,1.));
#6770=DIRECTION('ref_axis',(1.,0.,0.));
#6771=DIRECTION('axis',(0.,0.,1.));
#6772=DIRECTION('refdir',(1.,0.,0.));
#6773=DIRECTION('center_axis',(0.,0.,1.));
#6774=DIRECTION('ref_axis',(1.,0.,0.));
#6775=DIRECTION('center_axis',(0.,0.,-1.));
#6776=DIRECTION('ref_axis',(1.,0.,0.));
#6777=DIRECTION('',(0.,0.,-1.));
#6778=DIRECTION('center_axis',(0.,0.,-1.));
#6779=DIRECTION('ref_axis',(1.,0.,0.));
#6780=DIRECTION('center_axis',(0.,0.,1.));
#6781=DIRECTION('ref_axis',(1.,0.,0.));
#6782=DIRECTION('center_axis',(0.,0.,1.));
#6783=DIRECTION('ref_axis',(1.,0.,0.));
#6784=DIRECTION('',(0.,0.,-1.));
#6785=DIRECTION('center_axis',(0.,0.,1.));
#6786=DIRECTION('ref_axis',(1.,0.,0.));
#6787=DIRECTION('center_axis',(0.,0.,1.));
#6788=DIRECTION('ref_axis',(1.,0.,0.));
#6789=DIRECTION('center_axis',(0.,0.,1.));
#6790=DIRECTION('ref_axis',(1.,0.,0.));
#6791=DIRECTION('axis',(0.,0.,1.));
#6792=DIRECTION('refdir',(1.,0.,0.));
#6793=DIRECTION('center_axis',(0.866025403784439,0.,-0.5));
#6794=DIRECTION('ref_axis',(0.5,0.,0.866025403784439));
#6795=DIRECTION('',(-0.5,0.,-0.866025403784439));
#6796=DIRECTION('',(0.,-1.,0.));
#6797=DIRECTION('',(0.5,0.,0.866025403784439));
#6798=DIRECTION('',(0.,-1.,0.));
#6799=DIRECTION('center_axis',(1.60246890531964E-16,0.,-1.));
#6800=DIRECTION('ref_axis',(1.,0.,1.60246890531964E-16));
#6801=DIRECTION('',(-1.,0.,-1.60246890531964E-16));
#6802=DIRECTION('',(0.,-1.,0.));
#6803=DIRECTION('',(1.,0.,1.60246890531964E-16));
#6804=DIRECTION('center_axis',(-0.866025403784439,0.,-0.5));
#6805=DIRECTION('ref_axis',(0.5,0.,-0.866025403784439));
#6806=DIRECTION('',(-0.5,0.,0.866025403784439));
#6807=DIRECTION('',(0.,-1.,0.));
#6808=DIRECTION('',(0.5,0.,-0.866025403784439));
#6809=DIRECTION('center_axis',(-0.866025403784439,0.,0.5));
#6810=DIRECTION('ref_axis',(-0.5,0.,-0.866025403784439));
#6811=DIRECTION('',(0.5,0.,0.866025403784439));
#6812=DIRECTION('',(0.,-1.,0.));
#6813=DIRECTION('',(-0.5,0.,-0.866025403784439));
#6814=DIRECTION('center_axis',(-1.60246890531964E-16,0.,1.));
#6815=DIRECTION('ref_axis',(-1.,0.,-1.60246890531964E-16));
#6816=DIRECTION('',(1.,0.,1.60246890531964E-16));
#6817=DIRECTION('',(0.,-1.,0.));
#6818=DIRECTION('',(-1.,0.,-1.60246890531964E-16));
#6819=DIRECTION('center_axis',(0.866025403784439,0.,0.5));
#6820=DIRECTION('ref_axis',(-0.5,0.,0.866025403784439));
#6821=DIRECTION('',(0.5,0.,-0.866025403784439));
#6822=DIRECTION('',(-0.5,0.,0.866025403784439));
#6823=DIRECTION('center_axis',(0.,1.,0.));
#6824=DIRECTION('ref_axis',(1.,0.,0.));
#6825=DIRECTION('center_axis',(0.,-1.,0.));
#6826=DIRECTION('ref_axis',(0.,0.,-1.));
#6827=DIRECTION('center_axis',(0.,1.,0.));
#6828=DIRECTION('ref_axis',(1.,0.,0.));
#6829=DIRECTION('center_axis',(0.,1.,0.));
#6830=DIRECTION('ref_axis',(1.,0.,0.));
#6831=DIRECTION('center_axis',(0.,1.,0.));
#6832=DIRECTION('ref_axis',(0.,0.,1.));
#6833=DIRECTION('center_axis',(0.,-1.,0.));
#6834=DIRECTION('ref_axis',(1.,0.,0.));
#6835=DIRECTION('center_axis',(0.,-1.,0.));
#6836=DIRECTION('ref_axis',(1.,0.,0.));
#6837=DIRECTION('center_axis',(0.,-1.,0.));
#6838=DIRECTION('ref_axis',(1.,0.,0.));
#6839=DIRECTION('',(0.707106781186547,0.707106781186548,8.65956056235493E-17));
#6840=DIRECTION('center_axis',(0.,-1.,0.));
#6841=DIRECTION('ref_axis',(1.,0.,0.));
#6842=DIRECTION('center_axis',(0.,-1.,0.));
#6843=DIRECTION('ref_axis',(1.,0.,0.));
#6844=DIRECTION('',(0.,1.,0.));
#6845=DIRECTION('center_axis',(0.,1.,0.));
#6846=DIRECTION('ref_axis',(1.,0.,0.));
#6847=DIRECTION('center_axis',(0.,-1.,0.));
#6848=DIRECTION('ref_axis',(1.,0.,0.));
#6849=DIRECTION('',(-0.707106781186547,0.707106781186548,-8.65956056235493E-17));
#6850=DIRECTION('center_axis',(0.,-1.,0.));
#6851=DIRECTION('ref_axis',(0.,0.,-1.));
#6852=DIRECTION('center_axis',(0.,-1.,0.));
#6853=DIRECTION('ref_axis',(1.,0.,0.));
#6854=DIRECTION('center_axis',(0.,1.,0.));
#6855=DIRECTION('ref_axis',(1.,0.,0.));
#6856=DIRECTION('center_axis',(0.,1.,0.));
#6857=DIRECTION('ref_axis',(1.,0.,0.));
#6858=DIRECTION('',(-0.447213595499958,0.894427190999916,-5.47678698264203E-17));
#6859=DIRECTION('center_axis',(0.,-1.,0.));
#6860=DIRECTION('ref_axis',(1.,0.,0.));
#6861=DIRECTION('',(0.,1.,0.));
#6862=DIRECTION('',(0.,0.,1.));
#6863=DIRECTION('',(1.,0.,0.));
#6864=DIRECTION('',(0.,0.,1.));
#6865=DIRECTION('',(1.,0.,0.));
#6866=DIRECTION('',(0.,0.,1.));
#6867=DIRECTION('',(1.,0.,0.));
#6868=DIRECTION('',(0.,0.,1.));
#6869=DIRECTION('',(1.,0.,0.));
#6870=DIRECTION('',(0.,0.,1.));
#6871=DIRECTION('',(1.,0.,0.));
#6872=DIRECTION('',(0.,-1.,2.22044604925031E-16));
#6873=DIRECTION('',(1.,0.,0.));
#6874=DIRECTION('axis',(0.,0.,1.));
#6875=DIRECTION('refdir',(1.,0.,0.));
#6876=DIRECTION('axis',(0.,0.,1.));
#6877=DIRECTION('refdir',(1.,0.,0.));
#6878=DIRECTION('axis',(0.,0.,1.));
#6879=DIRECTION('refdir',(1.,0.,0.));
#6880=DIRECTION('center_axis',(0.,-1.,0.));
#6881=DIRECTION('ref_axis',(0.,0.,-1.));
#6882=DIRECTION('center_axis',(0.,-1.,0.));
#6883=DIRECTION('ref_axis',(1.,0.,0.));
#6884=DIRECTION('center_axis',(0.,-1.,0.));
#6885=DIRECTION('ref_axis',(1.,0.,0.));
#6886=DIRECTION('center_axis',(1.,0.,1.22464679914735E-16));
#6887=DIRECTION('ref_axis',(-1.22464679914735E-16,0.,1.));
#6888=DIRECTION('center_axis',(0.,1.,0.));
#6889=DIRECTION('ref_axis',(1.,0.,0.));
#6890=DIRECTION('center_axis',(0.,1.,0.));
#6891=DIRECTION('ref_axis',(1.,0.,0.));
#6892=DIRECTION('center_axis',(0.,-1.,0.));
#6893=DIRECTION('ref_axis',(1.,0.,0.));
#6894=DIRECTION('',(0.,1.,0.));
#6895=DIRECTION('center_axis',(0.,-1.,0.));
#6896=DIRECTION('ref_axis',(1.,0.,0.));
#6897=DIRECTION('center_axis',(0.,-1.,0.));
#6898=DIRECTION('ref_axis',(1.,0.,0.));
#6899=DIRECTION('center_axis',(0.,-1.,0.));
#6900=DIRECTION('ref_axis',(1.,0.,0.));
#6901=DIRECTION('',(0.,1.,0.));
#6902=DIRECTION('center_axis',(0.,-1.,0.));
#6903=DIRECTION('ref_axis',(1.,0.,0.));
#6904=DIRECTION('center_axis',(0.,1.,0.));
#6905=DIRECTION('ref_axis',(1.,0.,0.));
#6906=DIRECTION('',(-0.707106781186547,0.707106781186548,-8.65956056235493E-17));
#6907=DIRECTION('center_axis',(0.,-1.,0.));
#6908=DIRECTION('ref_axis',(1.,0.,0.));
#6909=DIRECTION('center_axis',(0.,1.,0.));
#6910=DIRECTION('ref_axis',(0.,0.,1.));
#6911=DIRECTION('center_axis',(0.,-1.,0.));
#6912=DIRECTION('ref_axis',(1.,0.,0.));
#6913=DIRECTION('center_axis',(0.,-1.,0.));
#6914=DIRECTION('ref_axis',(1.,0.,0.));
#6915=DIRECTION('',(0.,1.,0.));
#6916=DIRECTION('center_axis',(0.,-1.,0.));
#6917=DIRECTION('ref_axis',(0.,0.,-1.));
#6918=DIRECTION('center_axis',(0.,-1.,0.));
#6919=DIRECTION('ref_axis',(1.,0.,0.));
#6920=DIRECTION('center_axis',(0.,-1.,0.));
#6921=DIRECTION('ref_axis',(1.,0.,0.));
#6922=DIRECTION('',(0.707106781186547,0.707106781186548,8.65956056235493E-17));
#6923=DIRECTION('axis',(0.,0.,1.));
#6924=DIRECTION('refdir',(1.,0.,0.));
#6925=DIRECTION('center_axis',(0.,-1.,0.));
#6926=DIRECTION('ref_axis',(0.,0.,-1.));
#6927=DIRECTION('center_axis',(0.,-1.,0.));
#6928=DIRECTION('ref_axis',(1.,0.,0.));
#6929=DIRECTION('center_axis',(0.,-1.,0.));
#6930=DIRECTION('ref_axis',(1.,0.,0.));
#6931=DIRECTION('center_axis',(1.,0.,1.22464679914735E-16));
#6932=DIRECTION('ref_axis',(-1.22464679914735E-16,0.,1.));
#6933=DIRECTION('center_axis',(0.,1.,0.));
#6934=DIRECTION('ref_axis',(1.,0.,0.));
#6935=DIRECTION('center_axis',(0.,1.,0.));
#6936=DIRECTION('ref_axis',(1.,0.,0.));
#6937=DIRECTION('center_axis',(0.,-1.,0.));
#6938=DIRECTION('ref_axis',(1.,0.,0.));
#6939=DIRECTION('center_axis',(0.,-1.,0.));
#6940=DIRECTION('ref_axis',(1.,0.,0.));
#6941=DIRECTION('',(0.,1.,0.));
#6942=DIRECTION('center_axis',(0.,1.,0.));
#6943=DIRECTION('ref_axis',(0.,0.,1.));
#6944=DIRECTION('center_axis',(0.,-1.,0.));
#6945=DIRECTION('ref_axis',(1.,0.,0.));
#6946=DIRECTION('center_axis',(0.,-1.,0.));
#6947=DIRECTION('ref_axis',(1.,0.,0.));
#6948=DIRECTION('center_axis',(0.,-1.,0.));
#6949=DIRECTION('ref_axis',(1.,0.,0.));
#6950=DIRECTION('center_axis',(0.,-1.,0.));
#6951=DIRECTION('ref_axis',(1.,0.,0.));
#6952=DIRECTION('',(0.707106781186548,0.707106781186547,8.65956056235494E-17));
#6953=DIRECTION('center_axis',(0.,-1.,0.));
#6954=DIRECTION('ref_axis',(1.,0.,0.));
#6955=DIRECTION('center_axis',(0.,-1.,0.));
#6956=DIRECTION('ref_axis',(1.,0.,0.));
#6957=DIRECTION('',(0.,1.,0.));
#6958=DIRECTION('center_axis',(0.,1.,0.));
#6959=DIRECTION('ref_axis',(1.,0.,0.));
#6960=DIRECTION('center_axis',(0.,-1.,0.));
#6961=DIRECTION('ref_axis',(1.,0.,0.));
#6962=DIRECTION('',(-0.707106781186548,0.707106781186547,-8.65956056235494E-17));
#6963=DIRECTION('center_axis',(0.,-1.,0.));
#6964=DIRECTION('ref_axis',(0.,0.,-1.));
#6965=DIRECTION('center_axis',(0.,-1.,0.));
#6966=DIRECTION('ref_axis',(1.,0.,0.));
#6967=DIRECTION('',(0.,1.,0.));
#6968=DIRECTION('axis',(0.,0.,1.));
#6969=DIRECTION('refdir',(1.,0.,0.));
#6970=DIRECTION('center_axis',(0.,0.,1.));
#6971=DIRECTION('ref_axis',(1.,0.,0.));
#6972=DIRECTION('center_axis',(1.22464679914735E-16,-1.,0.));
#6973=DIRECTION('ref_axis',(-1.,-1.22464679914735E-16,0.));
#6974=DIRECTION('center_axis',(0.707106781186548,0.,0.707106781186548));
#6975=DIRECTION('ref_axis',(0.707106781186548,0.,-0.707106781186548));
#6976=DIRECTION('center_axis',(8.65956056235494E-17,-1.,-8.65956056235493E-17));
#6977=DIRECTION('ref_axis',(-0.707106781186547,-1.22464679914735E-16,0.707106781186547));
#6978=DIRECTION('center_axis',(1.,0.,0.));
#6979=DIRECTION('ref_axis',(6.12323399573676E-17,0.,-1.));
#6980=DIRECTION('center_axis',(7.49879891330929E-33,-1.,-1.22464679914735E-16));
#6981=DIRECTION('ref_axis',(-6.12323399573676E-17,-1.22464679914735E-16,
1.));
#6982=DIRECTION('center_axis',(0.707106781186548,0.,-0.707106781186548));
#6983=DIRECTION('ref_axis',(-0.707106781186548,0.,-0.707106781186548));
#6984=DIRECTION('center_axis',(-8.65956056235493E-17,-1.,-8.65956056235494E-17));
#6985=DIRECTION('ref_axis',(0.707106781186547,-1.22464679914735E-16,0.707106781186547));
#6986=DIRECTION('center_axis',(0.,0.,-1.));
#6987=DIRECTION('ref_axis',(-1.,0.,-1.22464679914735E-16));
#6988=DIRECTION('center_axis',(-1.22464679914735E-16,-1.,-1.49975978266186E-32));
#6989=DIRECTION('ref_axis',(1.,-1.22464679914735E-16,1.22464679914735E-16));
#6990=DIRECTION('center_axis',(-0.707106781186547,0.,-0.707106781186548));
#6991=DIRECTION('ref_axis',(-0.707106781186548,0.,0.707106781186547));
#6992=DIRECTION('center_axis',(-8.65956056235493E-17,-1.,8.65956056235493E-17));
#6993=DIRECTION('ref_axis',(0.707106781186548,-1.22464679914735E-16,-0.707106781186547));
#6994=DIRECTION('center_axis',(-1.,0.,0.));
#6995=DIRECTION('ref_axis',(-1.83697019872103E-16,0.,1.));
#6996=DIRECTION('center_axis',(-2.24963967399279E-32,-1.,1.22464679914735E-16));
#6997=DIRECTION('ref_axis',(1.83697019872103E-16,-1.22464679914735E-16,
-1.));
#6998=DIRECTION('center_axis',(-0.707106781186548,0.,0.707106781186548));
#6999=DIRECTION('ref_axis',(0.707106781186547,0.,0.707106781186548));
#7000=DIRECTION('center_axis',(8.65956056235493E-17,-1.,8.65956056235493E-17));
#7001=DIRECTION('ref_axis',(-0.707106781186547,-1.22464679914735E-16,-0.707106781186548));
#7002=DIRECTION('axis',(0.,0.,1.));
#7003=DIRECTION('refdir',(1.,0.,0.));
#7004=DIRECTION('center_axis',(0.,0.,1.));
#7005=DIRECTION('ref_axis',(1.,0.,0.));
#7006=DIRECTION('center_axis',(0.,-1.,0.));
#7007=DIRECTION('ref_axis',(0.,0.,-1.));
#7008=DIRECTION('center_axis',(0.,-1.,0.));
#7009=DIRECTION('ref_axis',(0.,0.,-1.));
#7010=DIRECTION('center_axis',(0.,1.,0.));
#7011=DIRECTION('ref_axis',(1.,0.,0.));
#7012=DIRECTION('center_axis',(0.,1.,0.));
#7013=DIRECTION('ref_axis',(1.,0.,0.));
#7014=DIRECTION('center_axis',(0.,1.,0.));
#7015=DIRECTION('ref_axis',(1.,0.,0.));
#7016=DIRECTION('center_axis',(0.,1.,0.));
#7017=DIRECTION('ref_axis',(1.,0.,0.));
#7018=DIRECTION('',(0.,-1.,0.));
#7019=DIRECTION('center_axis',(0.,-1.,0.));
#7020=DIRECTION('ref_axis',(1.,0.,0.));
#7021=DIRECTION('center_axis',(0.,1.,0.));
#7022=DIRECTION('ref_axis',(1.,0.,0.));
#7023=DIRECTION('center_axis',(0.,1.,0.));
#7024=DIRECTION('ref_axis',(1.,0.,0.));
#7025=DIRECTION('center_axis',(0.,1.,0.));
#7026=DIRECTION('ref_axis',(1.,0.,0.));
#7027=DIRECTION('center_axis',(0.,1.,0.));
#7028=DIRECTION('ref_axis',(1.,0.,0.));
#7029=DIRECTION('center_axis',(0.,1.,0.));
#7030=DIRECTION('ref_axis',(1.,0.,0.));
#7031=DIRECTION('center_axis',(0.,1.,0.));
#7032=DIRECTION('ref_axis',(1.,0.,0.));
#7033=DIRECTION('center_axis',(0.,-1.,0.));
#7034=DIRECTION('ref_axis',(1.,0.,0.));
#7035=DIRECTION('center_axis',(0.,-1.,0.));
#7036=DIRECTION('ref_axis',(0.,0.,-1.));
#7037=DIRECTION('center_axis',(6.12323399573677E-17,0.,1.));
#7038=DIRECTION('ref_axis',(1.,0.,0.));
#7039=DIRECTION('center_axis',(0.,-1.,0.));
#7040=DIRECTION('ref_axis',(0.,0.,-1.));
#7041=DIRECTION('center_axis',(0.,1.,0.));
#7042=DIRECTION('ref_axis',(1.,0.,0.));
#7043=DIRECTION('center_axis',(0.,-1.,0.));
#7044=DIRECTION('ref_axis',(1.,0.,0.));
#7045=DIRECTION('center_axis',(0.,-1.,0.));
#7046=DIRECTION('ref_axis',(0.,0.,-1.));
#7047=DIRECTION('center_axis',(0.,0.,1.));
#7048=DIRECTION('ref_axis',(1.,0.,0.));
#7049=DIRECTION('center_axis',(0.,-1.,0.));
#7050=DIRECTION('ref_axis',(0.,0.,-1.));
#7051=DIRECTION('center_axis',(0.,1.,0.));
#7052=DIRECTION('ref_axis',(1.,0.,0.));
#7053=DIRECTION('center_axis',(0.,-1.,0.));
#7054=DIRECTION('ref_axis',(1.,0.,0.));
#7055=DIRECTION('center_axis',(0.,-1.,0.));
#7056=DIRECTION('ref_axis',(0.,0.,-1.));
#7057=DIRECTION('center_axis',(0.,0.,1.));
#7058=DIRECTION('ref_axis',(1.,0.,0.));
#7059=DIRECTION('center_axis',(0.,-1.,0.));
#7060=DIRECTION('ref_axis',(0.,0.,-1.));
#7061=DIRECTION('center_axis',(0.,1.,0.));
#7062=DIRECTION('ref_axis',(1.,0.,0.));
#7063=DIRECTION('center_axis',(0.,-1.,0.));
#7064=DIRECTION('ref_axis',(1.,0.,0.));
#7065=DIRECTION('center_axis',(0.,-1.,0.));
#7066=DIRECTION('ref_axis',(0.,0.,-1.));
#7067=DIRECTION('center_axis',(0.,0.,1.));
#7068=DIRECTION('ref_axis',(1.,0.,0.));
#7069=DIRECTION('center_axis',(0.,-1.,0.));
#7070=DIRECTION('ref_axis',(0.,0.,-1.));
#7071=DIRECTION('center_axis',(0.,1.,0.));
#7072=DIRECTION('ref_axis',(1.,0.,0.));
#7073=DIRECTION('center_axis',(0.,-1.,0.));
#7074=DIRECTION('ref_axis',(1.,0.,0.));
#7075=DIRECTION('center_axis',(0.,-1.,0.));
#7076=DIRECTION('ref_axis',(0.,0.,-1.));
#7077=DIRECTION('center_axis',(6.12323399573676E-17,0.,1.));
#7078=DIRECTION('ref_axis',(1.,0.,0.));
#7079=DIRECTION('center_axis',(0.,-1.,0.));
#7080=DIRECTION('ref_axis',(0.,0.,-1.));
#7081=DIRECTION('center_axis',(0.,1.,0.));
#7082=DIRECTION('ref_axis',(1.,0.,0.));
#7083=DIRECTION('center_axis',(0.,-1.,0.));
#7084=DIRECTION('ref_axis',(1.,0.,0.));
#7085=DIRECTION('center_axis',(0.,-1.,0.));
#7086=DIRECTION('ref_axis',(0.,0.,-1.));
#7087=DIRECTION('center_axis',(0.,0.,1.));
#7088=DIRECTION('ref_axis',(1.,0.,0.));
#7089=DIRECTION('center_axis',(0.,-1.,0.));
#7090=DIRECTION('ref_axis',(0.,0.,-1.));
#7091=DIRECTION('center_axis',(0.,1.,0.));
#7092=DIRECTION('ref_axis',(1.,0.,0.));
#7093=DIRECTION('center_axis',(0.,1.,0.));
#7094=DIRECTION('ref_axis',(1.,0.,0.));
#7095=DIRECTION('',(0.,1.,0.));
#7096=DIRECTION('center_axis',(0.,-1.,0.));
#7097=DIRECTION('ref_axis',(1.,0.,0.));
#7098=DIRECTION('center_axis',(0.,-1.,0.));
#7099=DIRECTION('ref_axis',(1.,0.,0.));
#7100=DIRECTION('center_axis',(0.,1.,0.));
#7101=DIRECTION('ref_axis',(1.,0.,0.));
#7102=DIRECTION('center_axis',(0.,-1.,0.));
#7103=DIRECTION('ref_axis',(0.,0.,-1.));
#7104=DIRECTION('center_axis',(0.,0.,1.));
#7105=DIRECTION('ref_axis',(1.,0.,0.));
#7106=DIRECTION('center_axis',(0.,-1.,0.));
#7107=DIRECTION('ref_axis',(0.,0.,-1.));
#7108=DIRECTION('center_axis',(0.,-1.,0.));
#7109=DIRECTION('ref_axis',(-1.,0.,0.));
#7110=DIRECTION('center_axis',(0.,1.,0.));
#7111=DIRECTION('ref_axis',(1.,0.,0.));
#7112=DIRECTION('axis',(0.,0.,1.));
#7113=DIRECTION('refdir',(1.,0.,0.));
#7114=DIRECTION('center_axis',(0.,1.,0.));
#7115=DIRECTION('ref_axis',(0.,0.,1.));
#7116=DIRECTION('center_axis',(0.,-1.,0.));
#7117=DIRECTION('ref_axis',(1.,0.,0.));
#7118=DIRECTION('center_axis',(0.,-1.,0.));
#7119=DIRECTION('ref_axis',(1.,0.,0.));
#7120=DIRECTION('center_axis',(0.,-1.,0.));
#7121=DIRECTION('ref_axis',(1.,0.,0.));
#7122=DIRECTION('center_axis',(0.,-1.,0.));
#7123=DIRECTION('ref_axis',(1.,0.,0.));
#7124=DIRECTION('',(0.,1.,0.));
#7125=DIRECTION('center_axis',(0.,-1.,0.));
#7126=DIRECTION('ref_axis',(0.,0.,-1.));
#7127=DIRECTION('center_axis',(0.,-1.,0.));
#7128=DIRECTION('ref_axis',(1.,0.,0.));
#7129=DIRECTION('center_axis',(0.,-1.,0.));
#7130=DIRECTION('ref_axis',(1.,0.,0.));
#7131=DIRECTION('',(0.,1.,0.));
#7132=DIRECTION('center_axis',(0.,1.,0.));
#7133=DIRECTION('ref_axis',(0.,0.,1.));
#7134=DIRECTION('center_axis',(0.,-1.,0.));
#7135=DIRECTION('ref_axis',(1.,0.,0.));
#7136=DIRECTION('center_axis',(0.,-1.,0.));
#7137=DIRECTION('ref_axis',(1.,0.,0.));
#7138=DIRECTION('center_axis',(0.,-1.,0.));
#7139=DIRECTION('ref_axis',(1.,0.,0.));
#7140=DIRECTION('center_axis',(0.,-1.,0.));
#7141=DIRECTION('ref_axis',(1.,0.,0.));
#7142=DIRECTION('',(0.,1.,0.));
#7143=DIRECTION('center_axis',(0.,-1.,0.));
#7144=DIRECTION('ref_axis',(0.,0.,-1.));
#7145=DIRECTION('center_axis',(0.,-1.,0.));
#7146=DIRECTION('ref_axis',(1.,0.,0.));
#7147=DIRECTION('center_axis',(0.,-1.,0.));
#7148=DIRECTION('ref_axis',(1.,0.,0.));
#7149=DIRECTION('',(0.,1.,0.));
#7150=DIRECTION('',(0.,0.,1.));
#7151=DIRECTION('',(1.,0.,0.));
#7152=DIRECTION('',(0.,0.,1.));
#7153=DIRECTION('',(1.,0.,0.));
#7154=DIRECTION('',(0.,0.,1.));
#7155=DIRECTION('',(1.,0.,0.));
#7156=DIRECTION('',(0.,0.,1.));
#7157=DIRECTION('',(1.,0.,0.));
#7158=DIRECTION('',(0.,0.,1.));
#7159=DIRECTION('',(1.,0.,0.));
#7160=DIRECTION('',(0.,0.,1.));
#7161=DIRECTION('',(1.,0.,0.));
#7162=DIRECTION('',(0.,0.,1.));
#7163=DIRECTION('',(1.,0.,0.));
#7164=DIRECTION('',(0.,0.,1.));
#7165=DIRECTION('',(1.,0.,0.));
#7166=DIRECTION('',(0.,0.,1.));
#7167=DIRECTION('',(1.,0.,0.));
#7168=DIRECTION('',(0.,0.,1.));
#7169=DIRECTION('',(1.,0.,0.));
#7170=DIRECTION('',(0.,0.,1.));
#7171=DIRECTION('',(1.,0.,0.));
#7172=DIRECTION('',(0.,0.,1.));
#7173=DIRECTION('',(1.,0.,0.));
#7174=DIRECTION('',(0.,-1.,2.22044604925031E-16));
#7175=DIRECTION('',(1.,0.,0.));
#7176=DIRECTION('',(0.,-1.,2.22044604925031E-16));
#7177=DIRECTION('',(1.,0.,0.));
#7178=DIRECTION('',(0.,-1.,2.22044604925031E-16));
#7179=DIRECTION('',(1.,0.,0.));
#7180=DIRECTION('',(0.,-1.,2.22044604925031E-16));
#7181=DIRECTION('',(1.,0.,0.));
#7182=DIRECTION('',(0.,-1.,2.22044604925031E-16));
#7183=DIRECTION('',(1.,0.,0.));
#7184=DIRECTION('',(0.,-1.,2.22044604925031E-16));
#7185=DIRECTION('',(1.,0.,0.));
#7186=DIRECTION('',(0.,-1.,2.22044604925031E-16));
#7187=DIRECTION('',(1.,0.,0.));
#7188=DIRECTION('',(0.,-1.,2.22044604925031E-16));
#7189=DIRECTION('',(1.,0.,0.));
#7190=DIRECTION('',(0.,-1.,2.22044604925031E-16));
#7191=DIRECTION('',(1.,0.,0.));
#7192=DIRECTION('',(0.,0.,1.));
#7193=DIRECTION('',(2.22044604925031E-16,-1.,0.));
#7194=DIRECTION('',(0.,-1.,2.22044604925031E-16));
#7195=DIRECTION('',(1.,0.,0.));
#7196=DIRECTION('',(0.,-1.,2.22044604925031E-16));
#7197=DIRECTION('',(1.,0.,0.));
#7198=DIRECTION('',(0.,0.,1.));
#7199=DIRECTION('',(2.22044604925031E-16,1.,0.));
#7200=DIRECTION('',(0.,0.,1.));
#7201=DIRECTION('',(2.22044604925031E-16,1.,0.));
#7202=DIRECTION('',(0.,0.,1.));
#7203=DIRECTION('',(2.22044604925031E-16,1.,0.));
#7204=DIRECTION('',(0.,0.,1.));
#7205=DIRECTION('',(2.22044604925031E-16,1.,0.));
#7206=DIRECTION('',(0.,0.,1.));
#7207=DIRECTION('',(2.22044604925031E-16,-1.,0.));
#7208=DIRECTION('',(0.,0.,1.));
#7209=DIRECTION('',(2.22044604925031E-16,-1.,0.));
#7210=DIRECTION('',(0.,0.,1.));
#7211=DIRECTION('',(2.22044604925031E-16,-1.,0.));
#7212=DIRECTION('',(0.,0.,1.));
#7213=DIRECTION('',(2.22044604925031E-16,-1.,0.));
#7214=DIRECTION('',(0.,-1.,2.22044604925031E-16));
#7215=DIRECTION('',(1.,0.,0.));
#7216=DIRECTION('',(0.,0.,1.));
#7217=DIRECTION('',(1.,0.,0.));
#7218=DIRECTION('',(0.,0.,1.));
#7219=DIRECTION('',(-0.982941821691924,-0.183916761522602,0.));
#7220=DIRECTION('',(6.12323399573677E-17,-2.52542952382431E-48,1.));
#7221=DIRECTION('',(1.,1.54637959141184E-64,-6.12323399573677E-17));
#7222=DIRECTION('',(1.22464679914737E-16,-2.28704180895984E-33,1.00000000000001));
#7223=DIRECTION('',(0.807148537674574,0.590348404020702,-9.8847187309965E-17));
#7224=CARTESIAN_POINT('',(0.,0.,0.));
#7225=CARTESIAN_POINT('',(0.,0.,0.));
#7226=CARTESIAN_POINT('',(0.,0.,0.));
#7227=CARTESIAN_POINT('Origin',(10.7,1.5,-0.1));
#7228=CARTESIAN_POINT('',(10.49,1.5,0.));
#7229=CARTESIAN_POINT('Origin',(10.7,1.5,0.));
#7230=CARTESIAN_POINT('',(10.49,1.5,1.));
#7231=CARTESIAN_POINT('',(10.49,1.5,-0.1));
#7232=CARTESIAN_POINT('Origin',(10.7,1.5,1.));
#7233=CARTESIAN_POINT('Origin',(10.7,-1.5,-0.1));
#7234=CARTESIAN_POINT('',(10.49,-1.5,0.));
#7235=CARTESIAN_POINT('Origin',(10.7,-1.5,0.));
#7236=CARTESIAN_POINT('',(10.49,-1.5,1.));
#7237=CARTESIAN_POINT('',(10.49,-1.5,-0.1));
#7238=CARTESIAN_POINT('Origin',(10.7,-1.5,1.));
#7239=CARTESIAN_POINT('Origin',(1.76776695296637,-1.76776695296637,-0.1));
#7240=CARTESIAN_POINT('',(1.55776695296637,-1.76776695296637,0.));
#7241=CARTESIAN_POINT('Origin',(1.76776695296637,-1.76776695296637,0.));
#7242=CARTESIAN_POINT('',(1.55776695296637,-1.76776695296637,1.));
#7243=CARTESIAN_POINT('',(1.55776695296637,-1.76776695296637,-0.1));
#7244=CARTESIAN_POINT('Origin',(1.76776695296637,-1.76776695296637,1.));
#7245=CARTESIAN_POINT('Origin',(-1.76776695296637,-1.76776695296637,-0.1));
#7246=CARTESIAN_POINT('',(-1.97776695296637,-1.76776695296637,0.));
#7247=CARTESIAN_POINT('Origin',(-1.76776695296637,-1.76776695296637,0.));
#7248=CARTESIAN_POINT('',(-1.97776695296637,-1.76776695296637,1.));
#7249=CARTESIAN_POINT('',(-1.97776695296637,-1.76776695296637,-0.1));
#7250=CARTESIAN_POINT('Origin',(-1.76776695296637,-1.76776695296637,1.));
#7251=CARTESIAN_POINT('Origin',(-1.76776695296637,1.76776695296637,-0.1));
#7252=CARTESIAN_POINT('',(-1.97776695296637,1.76776695296637,0.));
#7253=CARTESIAN_POINT('Origin',(-1.76776695296637,1.76776695296637,0.));
#7254=CARTESIAN_POINT('',(-1.97776695296637,1.76776695296637,1.));
#7255=CARTESIAN_POINT('',(-1.97776695296637,1.76776695296637,-0.1));
#7256=CARTESIAN_POINT('Origin',(-1.76776695296637,1.76776695296637,1.));
#7257=CARTESIAN_POINT('Origin',(1.76776695296637,1.76776695296637,-0.1));
#7258=CARTESIAN_POINT('',(1.55776695296637,1.76776695296637,0.));
#7259=CARTESIAN_POINT('Origin',(1.76776695296637,1.76776695296637,0.));
#7260=CARTESIAN_POINT('',(1.55776695296637,1.76776695296637,1.));
#7261=CARTESIAN_POINT('',(1.55776695296637,1.76776695296637,-0.1));
#7262=CARTESIAN_POINT('Origin',(1.76776695296637,1.76776695296637,1.));
#7263=CARTESIAN_POINT('Origin',(11.5,5.,0.));
#7264=CARTESIAN_POINT('',(11.5,5.,0.));
#7265=CARTESIAN_POINT('',(-3.5,5.,0.));
#7266=CARTESIAN_POINT('',(11.5,5.,0.));
#7267=CARTESIAN_POINT('',(-3.5,5.,1.));
#7268=CARTESIAN_POINT('',(-3.5,5.,0.));
#7269=CARTESIAN_POINT('',(11.5,5.,1.));
#7270=CARTESIAN_POINT('',(11.5,5.,1.));
#7271=CARTESIAN_POINT('',(11.5,5.,0.));
#7272=CARTESIAN_POINT('Origin',(11.5,-5.,0.));
#7273=CARTESIAN_POINT('',(11.5,-5.,0.));
#7274=CARTESIAN_POINT('',(11.5,-5.,0.));
#7275=CARTESIAN_POINT('',(11.5,-5.,1.));
#7276=CARTESIAN_POINT('',(11.5,-5.,1.));
#7277=CARTESIAN_POINT('',(11.5,-5.,0.));
#7278=CARTESIAN_POINT('Origin',(-3.5,-5.,0.));
#7279=CARTESIAN_POINT('',(-3.5,-5.,0.));
#7280=CARTESIAN_POINT('',(-3.5,-5.,0.));
#7281=CARTESIAN_POINT('',(-3.5,-5.,1.));
#7282=CARTESIAN_POINT('',(-3.5,-5.,1.));
#7283=CARTESIAN_POINT('',(-3.5,-5.,0.));
#7284=CARTESIAN_POINT('Origin',(-3.5,5.,0.));
#7285=CARTESIAN_POINT('',(-3.5,5.,0.));
#7286=CARTESIAN_POINT('',(-3.5,5.,1.));
#7287=CARTESIAN_POINT('Origin',(4.,0.,1.));
#7288=CARTESIAN_POINT('Origin',(4.,0.,0.));
#7289=CARTESIAN_POINT('',(0.,0.,0.));
#7290=CARTESIAN_POINT('Origin',(11.5,0.,7.4));
#7291=CARTESIAN_POINT('',(10.,2.2,7.4));
#7292=CARTESIAN_POINT('',(10.,-2.2,7.4));
#7293=CARTESIAN_POINT('',(10.,2.,7.4));
#7294=CARTESIAN_POINT('',(13.,-2.2,7.4));
#7295=CARTESIAN_POINT('',(10.,-2.2,7.4));
#7296=CARTESIAN_POINT('',(13.,2.2,7.4));
#7297=CARTESIAN_POINT('',(13.,-2.,7.4));
#7298=CARTESIAN_POINT('',(13.,2.2,7.4));
#7299=CARTESIAN_POINT('',(10.2,1.5,7.4));
#7300=CARTESIAN_POINT('Origin',(10.7,1.5,7.4));
#7301=CARTESIAN_POINT('',(10.2,-1.5,7.4));
#7302=CARTESIAN_POINT('Origin',(10.7,-1.5,7.4));
#7303=CARTESIAN_POINT('Origin',(13.,2.2,1.));
#7304=CARTESIAN_POINT('',(13.,2.2,1.));
#7305=CARTESIAN_POINT('',(10.,2.2,1.));
#7306=CARTESIAN_POINT('',(13.,2.2,1.));
#7307=CARTESIAN_POINT('',(10.,2.2,1.));
#7308=CARTESIAN_POINT('',(13.,2.2,7.2));
#7309=CARTESIAN_POINT('Origin',(10.,-2.2,1.));
#7310=CARTESIAN_POINT('',(10.,-2.2,1.));
#7311=CARTESIAN_POINT('',(13.,-2.2,1.));
#7312=CARTESIAN_POINT('',(10.,-2.2,1.));
#7313=CARTESIAN_POINT('',(13.,-2.2,1.));
#7314=CARTESIAN_POINT('',(10.,-2.2,7.2));
#7315=CARTESIAN_POINT('Origin',(9.9,1.2,4.05));
#7316=CARTESIAN_POINT('',(10.,1.2,4.215));
#7317=CARTESIAN_POINT('Origin',(10.,1.2,4.05));
#7318=CARTESIAN_POINT('',(10.3,1.2,4.215));
#7319=CARTESIAN_POINT('',(9.9,1.2,4.215));
#7320=CARTESIAN_POINT('',(10.2185698389174,1.365,4.05));
#7321=CARTESIAN_POINT('Ctrl Pts',(10.2185698389174,1.365,4.05));
#7322=CARTESIAN_POINT('Ctrl Pts',(10.2185698389174,1.365,4.02952043356281));
#7323=CARTESIAN_POINT('Ctrl Pts',(10.2196511820674,1.360940751691,4.00771516465356));
#7324=CARTESIAN_POINT('Ctrl Pts',(10.2246631762912,1.34467012765305,3.96777784587771));
#7325=CARTESIAN_POINT('Ctrl Pts',(10.2286736827823,1.33246344039378,3.94965394795779));
#7326=CARTESIAN_POINT('Ctrl Pts',(10.2402354326321,1.30274117773169,3.91885215023316));
#7327=CARTESIAN_POINT('Ctrl Pts',(10.2490773513426,1.28266254990227,3.90542718243916));
#7328=CARTESIAN_POINT('Ctrl Pts',(10.2717677906972,1.24080126498159,3.8885390180969));
#7329=CARTESIAN_POINT('Ctrl Pts',(10.2856850788648,1.21908656151361,3.885));
#7330=CARTESIAN_POINT('Ctrl Pts',(10.319085409969,1.17455278670803,3.885));
#7331=CARTESIAN_POINT('Ctrl Pts',(10.3419048713612,1.14954238521319,3.89106755072681));
#7332=CARTESIAN_POINT('Ctrl Pts',(10.3901989916138,1.10620312192356,3.91213177324836));
#7333=CARTESIAN_POINT('Ctrl Pts',(10.415674165106,1.08782446907905,3.92702466368572));
#7334=CARTESIAN_POINT('Ctrl Pts',(10.4559623955469,1.06313017986469,3.95639578484302));
#7335=CARTESIAN_POINT('Ctrl Pts',(10.4744285153863,1.05346991878665,3.97182573634243));
#7336=CARTESIAN_POINT('Ctrl Pts',(10.4968465722861,1.04305739521201,3.99819879372234));
#7337=CARTESIAN_POINT('Ctrl Pts',(10.5033924526994,1.04024696261202,4.00748456076932));
#7338=CARTESIAN_POINT('Ctrl Pts',(10.5130578430487,1.03623280243464,4.02744119259084));
#7339=CARTESIAN_POINT('Ctrl Pts',(10.5162202405051,1.035,4.03808539531883));
#7340=CARTESIAN_POINT('Ctrl Pts',(10.5162202405051,1.035,4.06191460468117));
#7341=CARTESIAN_POINT('Ctrl Pts',(10.5130578430487,1.03623280243464,4.07255880740916));
#7342=CARTESIAN_POINT('Ctrl Pts',(10.5033924526994,1.04024696261203,4.09251543923068));
#7343=CARTESIAN_POINT('Ctrl Pts',(10.4968465722861,1.04305739521201,4.10180120627766));
#7344=CARTESIAN_POINT('Ctrl Pts',(10.4744285153863,1.05346991878665,4.12817426365757));
#7345=CARTESIAN_POINT('Ctrl Pts',(10.4559623955469,1.06313017986469,4.14360421515698));
#7346=CARTESIAN_POINT('Ctrl Pts',(10.415674165106,1.08782446907905,4.17297533631428));
#7347=CARTESIAN_POINT('Ctrl Pts',(10.3901989916138,1.10620312192356,4.18786822675164));
#7348=CARTESIAN_POINT('Ctrl Pts',(10.3419048713612,1.14954238521319,4.20893244927319));
#7349=CARTESIAN_POINT('Ctrl Pts',(10.319085409969,1.17455278670803,4.215));
#7350=CARTESIAN_POINT('Ctrl Pts',(10.3,1.2,4.215));
#7351=CARTESIAN_POINT('Ctrl Pts',(10.3,1.2,4.215));
#7352=CARTESIAN_POINT('Ctrl Pts',(10.2856850788648,1.21908656151361,4.215));
#7353=CARTESIAN_POINT('Ctrl Pts',(10.2717677906972,1.24080126498159,4.2114609819031));
#7354=CARTESIAN_POINT('Ctrl Pts',(10.2490773513426,1.28266254990227,4.19457281756084));
#7355=CARTESIAN_POINT('Ctrl Pts',(10.2402354326322,1.30274117773169,4.18114784976684));
#7356=CARTESIAN_POINT('Ctrl Pts',(10.2286736827823,1.33246344039378,4.15034605204221));
#7357=CARTESIAN_POINT('Ctrl Pts',(10.2246631762912,1.34467012765305,4.13222215412229));
#7358=CARTESIAN_POINT('Ctrl Pts',(10.2196511820674,1.360940751691,4.09228483534644));
#7359=CARTESIAN_POINT('Ctrl Pts',(10.2185698389174,1.365,4.07047956643719));
#7360=CARTESIAN_POINT('Ctrl Pts',(10.2185698389174,1.365,4.05));
#7361=CARTESIAN_POINT('Origin',(9.9,1.2,4.05));
#7362=CARTESIAN_POINT('',(11.1814301610826,1.365,4.05));
#7363=CARTESIAN_POINT('',(11.1,1.2,4.215));
#7364=CARTESIAN_POINT('Ctrl Pts',(11.1814301610826,1.365,4.05));
#7365=CARTESIAN_POINT('Ctrl Pts',(11.1814301610826,1.365,4.07047956643719));
#7366=CARTESIAN_POINT('Ctrl Pts',(11.1803488179326,1.360940751691,4.09228483534644));
#7367=CARTESIAN_POINT('Ctrl Pts',(11.1753368237088,1.34467012765305,4.13222215412229));
#7368=CARTESIAN_POINT('Ctrl Pts',(11.1713263172177,1.33246344039378,4.15034605204221));
#7369=CARTESIAN_POINT('Ctrl Pts',(11.1597645673678,1.30274117773169,4.18114784976684));
#7370=CARTESIAN_POINT('Ctrl Pts',(11.1509226486574,1.28266254990227,4.19457281756084));
#7371=CARTESIAN_POINT('Ctrl Pts',(11.1282322093028,1.24080126498159,4.2114609819031));
#7372=CARTESIAN_POINT('Ctrl Pts',(11.1143149211352,1.21908656151361,4.215));
#7373=CARTESIAN_POINT('Ctrl Pts',(11.1,1.2,4.215));
#7374=CARTESIAN_POINT('Ctrl Pts',(11.1,1.2,4.215));
#7375=CARTESIAN_POINT('Ctrl Pts',(11.080914590031,1.17455278670802,4.215));
#7376=CARTESIAN_POINT('Ctrl Pts',(11.0580951286388,1.14954238521319,4.20893244927319));
#7377=CARTESIAN_POINT('Ctrl Pts',(11.0098010083862,1.10620312192356,4.18786822675164));
#7378=CARTESIAN_POINT('Ctrl Pts',(10.984325834894,1.08782446907905,4.17297533631428));
#7379=CARTESIAN_POINT('Ctrl Pts',(10.9440376044531,1.06313017986469,4.14360421515698));
#7380=CARTESIAN_POINT('Ctrl Pts',(10.9255714846137,1.05346991878665,4.12817426365757));
#7381=CARTESIAN_POINT('Ctrl Pts',(10.9031534277139,1.04305739521201,4.10180120627766));
#7382=CARTESIAN_POINT('Ctrl Pts',(10.8966075473006,1.04024696261203,4.09251543923068));
#7383=CARTESIAN_POINT('Ctrl Pts',(10.8869421569513,1.03623280243464,4.07255880740916));
#7384=CARTESIAN_POINT('Ctrl Pts',(10.8837797594949,1.035,4.06191460468117));
#7385=CARTESIAN_POINT('Ctrl Pts',(10.8837797594949,1.035,4.03808539531883));
#7386=CARTESIAN_POINT('Ctrl Pts',(10.8869421569513,1.03623280243464,4.02744119259084));
#7387=CARTESIAN_POINT('Ctrl Pts',(10.8966075473006,1.04024696261202,4.00748456076932));
#7388=CARTESIAN_POINT('Ctrl Pts',(10.9031534277139,1.04305739521201,3.99819879372234));
#7389=CARTESIAN_POINT('Ctrl Pts',(10.9255714846137,1.05346991878665,3.97182573634243));
#7390=CARTESIAN_POINT('Ctrl Pts',(10.9440376044531,1.06313017986469,3.95639578484302));
#7391=CARTESIAN_POINT('Ctrl Pts',(10.984325834894,1.08782446907905,3.92702466368572));
#7392=CARTESIAN_POINT('Ctrl Pts',(11.0098010083862,1.10620312192356,3.91213177324836));
#7393=CARTESIAN_POINT('Ctrl Pts',(11.0580951286388,1.14954238521319,3.89106755072681));
#7394=CARTESIAN_POINT('Ctrl Pts',(11.080914590031,1.17455278670803,3.885));
#7395=CARTESIAN_POINT('Ctrl Pts',(11.1143149211352,1.21908656151361,3.885));
#7396=CARTESIAN_POINT('Ctrl Pts',(11.1282322093028,1.24080126498159,3.8885390180969));
#7397=CARTESIAN_POINT('Ctrl Pts',(11.1509226486574,1.28266254990227,3.90542718243916));
#7398=CARTESIAN_POINT('Ctrl Pts',(11.1597645673678,1.30274117773169,3.91885215023316));
#7399=CARTESIAN_POINT('Ctrl Pts',(11.1713263172177,1.33246344039378,3.94965394795779));
#7400=CARTESIAN_POINT('Ctrl Pts',(11.1753368237088,1.34467012765305,3.96777784587771));
#7401=CARTESIAN_POINT('Ctrl Pts',(11.1803488179326,1.360940751691,4.00771516465356));
#7402=CARTESIAN_POINT('Ctrl Pts',(11.1814301610826,1.365,4.02952043356281));
#7403=CARTESIAN_POINT('Ctrl Pts',(11.1814301610826,1.365,4.05));
#7404=CARTESIAN_POINT('',(13.,1.2,4.215));
#7405=CARTESIAN_POINT('',(9.9,1.2,4.215));
#7406=CARTESIAN_POINT('Origin',(13.,1.2,4.05));
#7407=CARTESIAN_POINT('Origin',(9.9,-1.2,6.45));
#7408=CARTESIAN_POINT('',(10.,-1.2,6.615));
#7409=CARTESIAN_POINT('Origin',(10.,-1.2,6.45));
#7410=CARTESIAN_POINT('',(10.3,-1.2,6.615));
#7411=CARTESIAN_POINT('',(9.9,-1.2,6.615));
#7412=CARTESIAN_POINT('',(10.5162202405051,-1.035,6.45));
#7413=CARTESIAN_POINT('Ctrl Pts',(10.5162202405051,-1.035,6.45));
#7414=CARTESIAN_POINT('Ctrl Pts',(10.5162202405051,-1.035,6.44062045354281));
#7415=CARTESIAN_POINT('Ctrl Pts',(10.5140205633862,-1.0358566636217,6.43083371614971));
#7416=CARTESIAN_POINT('Ctrl Pts',(10.5063054900173,-1.03902296892558,6.41262650433697));
#7417=CARTESIAN_POINT('Ctrl Pts',(10.5008967482507,-1.04131297855552,6.4041576160186));
#7418=CARTESIAN_POINT('Ctrl Pts',(10.4762824962743,-1.05234965200392,6.37165968077989));
#7419=CARTESIAN_POINT('Ctrl Pts',(10.4475863157778,-1.0674330397717,6.34922172243674));
#7420=CARTESIAN_POINT('Ctrl Pts',(10.4028942700183,-1.09707700316755,6.31957775904089));
#7421=CARTESIAN_POINT('Ctrl Pts',(10.3802569440026,-1.11447899483743,6.30721461318364));
#7422=CARTESIAN_POINT('Ctrl Pts',(10.3373328915009,-1.15455153425976,6.28988771813691));
#7423=CARTESIAN_POINT('Ctrl Pts',(10.3170531808664,-1.17726242551144,6.285));
#7424=CARTESIAN_POINT('Ctrl Pts',(10.2859943020946,-1.21867426387382,6.285));
#7425=CARTESIAN_POINT('Ctrl Pts',(10.2723294055107,-1.2399125795835,6.28838530514966));
#7426=CARTESIAN_POINT('Ctrl Pts',(10.249906982231,-1.28099344112303,6.30456138651949));
#7427=CARTESIAN_POINT('Ctrl Pts',(10.2410876841917,-1.30077258467692,6.31742734688536));
#7428=CARTESIAN_POINT('Ctrl Pts',(10.2291861979204,-1.33097165226366,6.3476264144721));
#7429=CARTESIAN_POINT('Ctrl Pts',(10.2249675898062,-1.34371971020651,6.36599964223317));
#7430=CARTESIAN_POINT('Ctrl Pts',(10.2197033363378,-1.36073611264639,6.40669500858237));
#7431=CARTESIAN_POINT('Ctrl Pts',(10.2185698389174,-1.365,6.42900759846042));
#7432=CARTESIAN_POINT('Ctrl Pts',(10.2185698389174,-1.365,6.47047956643719));
#7433=CARTESIAN_POINT('Ctrl Pts',(10.2196511820674,-1.360940751691,6.49228483534644));
#7434=CARTESIAN_POINT('Ctrl Pts',(10.2246631762912,-1.34467012765305,6.53222215412229));
#7435=CARTESIAN_POINT('Ctrl Pts',(10.2286736827823,-1.33246344039378,6.55034605204221));
#7436=CARTESIAN_POINT('Ctrl Pts',(10.2402354326322,-1.30274117773169,6.58114784976684));
#7437=CARTESIAN_POINT('Ctrl Pts',(10.2490773513426,-1.28266254990227,6.59457281756084));
#7438=CARTESIAN_POINT('Ctrl Pts',(10.2717677906972,-1.24080126498159,6.6114609819031));
#7439=CARTESIAN_POINT('Ctrl Pts',(10.2856850788648,-1.21908656151361,6.615));
#7440=CARTESIAN_POINT('Ctrl Pts',(10.3,-1.2,6.615));
#7441=CARTESIAN_POINT('Ctrl Pts',(10.3,-1.2,6.615));
#7442=CARTESIAN_POINT('Ctrl Pts',(10.319085409969,-1.17455278670802,6.615));
#7443=CARTESIAN_POINT('Ctrl Pts',(10.3419048713612,-1.14954238521319,6.60893244927319));
#7444=CARTESIAN_POINT('Ctrl Pts',(10.3901989916138,-1.10620312192356,6.58786822675164));
#7445=CARTESIAN_POINT('Ctrl Pts',(10.415674165106,-1.08782446907905,6.57297533631428));
#7446=CARTESIAN_POINT('Ctrl Pts',(10.4559623955469,-1.06313017986469,6.54360421515698));
#7447=CARTESIAN_POINT('Ctrl Pts',(10.4744285153863,-1.05346991878665,6.52817426365758));
#7448=CARTESIAN_POINT('Ctrl Pts',(10.4968465722861,-1.04305739521201,6.50180120627766));
#7449=CARTESIAN_POINT('Ctrl Pts',(10.5033924526994,-1.04024696261203,6.49251543923068));
#7450=CARTESIAN_POINT('Ctrl Pts',(10.5130578430487,-1.03623280243464,6.47255880740916));
#7451=CARTESIAN_POINT('Ctrl Pts',(10.5162202405051,-1.035,6.46191460468117));
#7452=CARTESIAN_POINT('Ctrl Pts',(10.5162202405051,-1.035,6.45));
#7453=CARTESIAN_POINT('Origin',(9.9,-1.2,6.45));
#7454=CARTESIAN_POINT('',(10.8837797594949,-1.035,6.45));
#7455=CARTESIAN_POINT('',(11.1,-1.2,6.615));
#7456=CARTESIAN_POINT('Ctrl Pts',(10.8837797594949,-1.035,6.45));
#7457=CARTESIAN_POINT('Ctrl Pts',(10.8837797594949,-1.035,6.46191460468117));
#7458=CARTESIAN_POINT('Ctrl Pts',(10.8869421569513,-1.03623280243464,6.47255880740916));
#7459=CARTESIAN_POINT('Ctrl Pts',(10.8966075473006,-1.04024696261203,6.49251543923068));
#7460=CARTESIAN_POINT('Ctrl Pts',(10.9031534277139,-1.04305739521201,6.50180120627766));
#7461=CARTESIAN_POINT('Ctrl Pts',(10.9255714846137,-1.05346991878665,6.52817426365758));
#7462=CARTESIAN_POINT('Ctrl Pts',(10.9440376044531,-1.06313017986469,6.54360421515698));
#7463=CARTESIAN_POINT('Ctrl Pts',(10.984325834894,-1.08782446907905,6.57297533631428));
#7464=CARTESIAN_POINT('Ctrl Pts',(11.0098010083862,-1.10620312192356,6.58786822675164));
#7465=CARTESIAN_POINT('Ctrl Pts',(11.0580951286388,-1.14954238521319,6.60893244927319));
#7466=CARTESIAN_POINT('Ctrl Pts',(11.080914590031,-1.17455278670802,6.615));
#7467=CARTESIAN_POINT('Ctrl Pts',(11.1,-1.2,6.615));
#7468=CARTESIAN_POINT('Ctrl Pts',(11.1,-1.2,6.615));
#7469=CARTESIAN_POINT('Ctrl Pts',(11.1143149211352,-1.21908656151361,6.615));
#7470=CARTESIAN_POINT('Ctrl Pts',(11.1282322093028,-1.24080126498159,6.6114609819031));
#7471=CARTESIAN_POINT('Ctrl Pts',(11.1509226486574,-1.28266254990227,6.59457281756084));
#7472=CARTESIAN_POINT('Ctrl Pts',(11.1597645673678,-1.30274117773169,6.58114784976684));
#7473=CARTESIAN_POINT('Ctrl Pts',(11.1713263172177,-1.33246344039378,6.55034605204221));
#7474=CARTESIAN_POINT('Ctrl Pts',(11.1753368237088,-1.34467012765305,6.53222215412229));
#7475=CARTESIAN_POINT('Ctrl Pts',(11.1803488179326,-1.360940751691,6.49228483534644));
#7476=CARTESIAN_POINT('Ctrl Pts',(11.1814301610826,-1.365,6.47047956643719));
#7477=CARTESIAN_POINT('Ctrl Pts',(11.1814301610826,-1.365,6.42900759846042));
#7478=CARTESIAN_POINT('Ctrl Pts',(11.1802966636622,-1.36073611264639,6.40669500858237));
#7479=CARTESIAN_POINT('Ctrl Pts',(11.1750324101937,-1.34371971020651,6.36599964223317));
#7480=CARTESIAN_POINT('Ctrl Pts',(11.1708138020796,-1.33097165226366,6.3476264144721));
#7481=CARTESIAN_POINT('Ctrl Pts',(11.1589123158083,-1.30077258467692,6.31742734688536));
#7482=CARTESIAN_POINT('Ctrl Pts',(11.150093017769,-1.28099344112303,6.30456138651949));
#7483=CARTESIAN_POINT('Ctrl Pts',(11.1276705944893,-1.23991257958351,6.28838530514966));
#7484=CARTESIAN_POINT('Ctrl Pts',(11.1140056979054,-1.21867426387382,6.285));
#7485=CARTESIAN_POINT('Ctrl Pts',(11.0829468191336,-1.17726242551144,6.285));
#7486=CARTESIAN_POINT('Ctrl Pts',(11.0626671084991,-1.15455153425976,6.28988771813691));
#7487=CARTESIAN_POINT('Ctrl Pts',(11.0197430559974,-1.11447899483743,6.30721461318364));
#7488=CARTESIAN_POINT('Ctrl Pts',(10.9971057299817,-1.09707700316755,6.31957775904089));
#7489=CARTESIAN_POINT('Ctrl Pts',(10.9524136842222,-1.0674330397717,6.34922172243674));
#7490=CARTESIAN_POINT('Ctrl Pts',(10.9237175037257,-1.05234965200392,6.37165968077989));
#7491=CARTESIAN_POINT('Ctrl Pts',(10.8991032517493,-1.04131297855552,6.4041576160186));
#7492=CARTESIAN_POINT('Ctrl Pts',(10.8936945099827,-1.03902296892558,6.41262650433697));
#7493=CARTESIAN_POINT('Ctrl Pts',(10.8859794366138,-1.0358566636217,6.43083371614971));
#7494=CARTESIAN_POINT('Ctrl Pts',(10.8837797594949,-1.035,6.44062045354281));
#7495=CARTESIAN_POINT('Ctrl Pts',(10.8837797594949,-1.035,6.45));
#7496=CARTESIAN_POINT('',(13.,-1.2,6.615));
#7497=CARTESIAN_POINT('',(9.9,-1.2,6.615));
#7498=CARTESIAN_POINT('Origin',(13.,-1.2,6.45));
#7499=CARTESIAN_POINT('Origin',(9.9,-1.2,4.05));
#7500=CARTESIAN_POINT('',(10.,-1.2,4.215));
#7501=CARTESIAN_POINT('Origin',(10.,-1.2,4.05));
#7502=CARTESIAN_POINT('',(10.3,-1.2,4.215));
#7503=CARTESIAN_POINT('',(9.9,-1.2,4.215));
#7504=CARTESIAN_POINT('',(10.5162202405051,-1.035,4.05));
#7505=CARTESIAN_POINT('Ctrl Pts',(10.5162202405051,-1.035,4.05));
#7506=CARTESIAN_POINT('Ctrl Pts',(10.5162202405051,-1.035,4.03808539531883));
#7507=CARTESIAN_POINT('Ctrl Pts',(10.5130578430487,-1.03623280243464,4.02744119259084));
#7508=CARTESIAN_POINT('Ctrl Pts',(10.5033924526994,-1.04024696261202,4.00748456076932));
#7509=CARTESIAN_POINT('Ctrl Pts',(10.4968465722861,-1.04305739521201,3.99819879372234));
#7510=CARTESIAN_POINT('Ctrl Pts',(10.4744285153863,-1.05346991878665,3.97182573634243));
#7511=CARTESIAN_POINT('Ctrl Pts',(10.4559623955469,-1.06313017986469,3.95639578484302));
#7512=CARTESIAN_POINT('Ctrl Pts',(10.415674165106,-1.08782446907905,3.92702466368572));
#7513=CARTESIAN_POINT('Ctrl Pts',(10.3901989916138,-1.10620312192356,3.91213177324836));
#7514=CARTESIAN_POINT('Ctrl Pts',(10.3419048713612,-1.14954238521319,3.89106755072681));
#7515=CARTESIAN_POINT('Ctrl Pts',(10.319085409969,-1.17455278670803,3.885));
#7516=CARTESIAN_POINT('Ctrl Pts',(10.2856850788648,-1.21908656151361,3.885));
#7517=CARTESIAN_POINT('Ctrl Pts',(10.2717677906972,-1.24080126498159,3.88853901809689));
#7518=CARTESIAN_POINT('Ctrl Pts',(10.2490773513426,-1.28266254990227,3.90542718243916));
#7519=CARTESIAN_POINT('Ctrl Pts',(10.2402354326321,-1.30274117773169,3.91885215023316));
#7520=CARTESIAN_POINT('Ctrl Pts',(10.2286736827823,-1.33246344039378,3.94965394795779));
#7521=CARTESIAN_POINT('Ctrl Pts',(10.2246631762912,-1.34467012765305,3.96777784587771));
#7522=CARTESIAN_POINT('Ctrl Pts',(10.2196511820674,-1.360940751691,4.00771516465356));
#7523=CARTESIAN_POINT('Ctrl Pts',(10.2185698389174,-1.365,4.02952043356281));
#7524=CARTESIAN_POINT('Ctrl Pts',(10.2185698389174,-1.365,4.07047956643719));
#7525=CARTESIAN_POINT('Ctrl Pts',(10.2196511820674,-1.360940751691,4.09228483534644));
#7526=CARTESIAN_POINT('Ctrl Pts',(10.2246631762912,-1.34467012765305,4.13222215412229));
#7527=CARTESIAN_POINT('Ctrl Pts',(10.2286736827823,-1.33246344039378,4.15034605204221));
#7528=CARTESIAN_POINT('Ctrl Pts',(10.2402354326321,-1.30274117773169,4.18114784976684));
#7529=CARTESIAN_POINT('Ctrl Pts',(10.2490773513426,-1.28266254990227,4.19457281756084));
#7530=CARTESIAN_POINT('Ctrl Pts',(10.2717677906972,-1.24080126498159,4.2114609819031));
#7531=CARTESIAN_POINT('Ctrl Pts',(10.2856850788648,-1.21908656151361,4.215));
#7532=CARTESIAN_POINT('Ctrl Pts',(10.3,-1.2,4.215));
#7533=CARTESIAN_POINT('Ctrl Pts',(10.3,-1.2,4.215));
#7534=CARTESIAN_POINT('Ctrl Pts',(10.319085409969,-1.17455278670802,4.215));
#7535=CARTESIAN_POINT('Ctrl Pts',(10.3419048713612,-1.14954238521319,4.20893244927319));
#7536=CARTESIAN_POINT('Ctrl Pts',(10.3901989916138,-1.10620312192356,4.18786822675164));
#7537=CARTESIAN_POINT('Ctrl Pts',(10.415674165106,-1.08782446907905,4.17297533631428));
#7538=CARTESIAN_POINT('Ctrl Pts',(10.4559623955469,-1.06313017986469,4.14360421515698));
#7539=CARTESIAN_POINT('Ctrl Pts',(10.4744285153863,-1.05346991878665,4.12817426365757));
#7540=CARTESIAN_POINT('Ctrl Pts',(10.4968465722861,-1.04305739521201,4.10180120627766));
#7541=CARTESIAN_POINT('Ctrl Pts',(10.5033924526994,-1.04024696261203,4.09251543923068));
#7542=CARTESIAN_POINT('Ctrl Pts',(10.5130578430487,-1.03623280243464,4.07255880740916));
#7543=CARTESIAN_POINT('Ctrl Pts',(10.5162202405051,-1.035,4.06191460468117));
#7544=CARTESIAN_POINT('Ctrl Pts',(10.5162202405051,-1.035,4.05));
#7545=CARTESIAN_POINT('Origin',(9.9,-1.2,4.05));
#7546=CARTESIAN_POINT('',(10.8837797594949,-1.035,4.05));
#7547=CARTESIAN_POINT('',(11.1,-1.2,4.215));
#7548=CARTESIAN_POINT('Ctrl Pts',(10.8837797594949,-1.035,4.05));
#7549=CARTESIAN_POINT('Ctrl Pts',(10.8837797594949,-1.035,4.06191460468117));
#7550=CARTESIAN_POINT('Ctrl Pts',(10.8869421569513,-1.03623280243464,4.07255880740916));
#7551=CARTESIAN_POINT('Ctrl Pts',(10.8966075473006,-1.04024696261203,4.09251543923068));
#7552=CARTESIAN_POINT('Ctrl Pts',(10.9031534277139,-1.04305739521201,4.10180120627766));
#7553=CARTESIAN_POINT('Ctrl Pts',(10.9255714846137,-1.05346991878665,4.12817426365757));
#7554=CARTESIAN_POINT('Ctrl Pts',(10.9440376044531,-1.06313017986469,4.14360421515698));
#7555=CARTESIAN_POINT('Ctrl Pts',(10.984325834894,-1.08782446907905,4.17297533631428));
#7556=CARTESIAN_POINT('Ctrl Pts',(11.0098010083862,-1.10620312192355,4.18786822675163));
#7557=CARTESIAN_POINT('Ctrl Pts',(11.0580951286388,-1.14954238521319,4.20893244927319));
#7558=CARTESIAN_POINT('Ctrl Pts',(11.080914590031,-1.17455278670803,4.215));
#7559=CARTESIAN_POINT('Ctrl Pts',(11.1,-1.2,4.215));
#7560=CARTESIAN_POINT('Ctrl Pts',(11.1,-1.2,4.215));
#7561=CARTESIAN_POINT('Ctrl Pts',(11.1143149211352,-1.21908656151361,4.215));
#7562=CARTESIAN_POINT('Ctrl Pts',(11.1282322093028,-1.24080126498159,4.2114609819031));
#7563=CARTESIAN_POINT('Ctrl Pts',(11.1509226486574,-1.28266254990227,4.19457281756084));
#7564=CARTESIAN_POINT('Ctrl Pts',(11.1597645673678,-1.30274117773169,4.18114784976684));
#7565=CARTESIAN_POINT('Ctrl Pts',(11.1713263172177,-1.33246344039378,4.15034605204221));
#7566=CARTESIAN_POINT('Ctrl Pts',(11.1753368237088,-1.34467012765305,4.13222215412229));
#7567=CARTESIAN_POINT('Ctrl Pts',(11.1803488179326,-1.360940751691,4.09228483534644));
#7568=CARTESIAN_POINT('Ctrl Pts',(11.1814301610826,-1.365,4.07047956643719));
#7569=CARTESIAN_POINT('Ctrl Pts',(11.1814301610826,-1.365,4.02952043356281));
#7570=CARTESIAN_POINT('Ctrl Pts',(11.1803488179326,-1.360940751691,4.00771516465356));
#7571=CARTESIAN_POINT('Ctrl Pts',(11.1753368237088,-1.34467012765305,3.96777784587771));
#7572=CARTESIAN_POINT('Ctrl Pts',(11.1713263172177,-1.33246344039378,3.94965394795779));
#7573=CARTESIAN_POINT('Ctrl Pts',(11.1597645673678,-1.30274117773169,3.91885215023316));
#7574=CARTESIAN_POINT('Ctrl Pts',(11.1509226486574,-1.28266254990227,3.90542718243916));
#7575=CARTESIAN_POINT('Ctrl Pts',(11.1282322093028,-1.24080126498159,3.8885390180969));
#7576=CARTESIAN_POINT('Ctrl Pts',(11.1143149211352,-1.21908656151361,3.885));
#7577=CARTESIAN_POINT('Ctrl Pts',(11.080914590031,-1.17455278670803,3.885));
#7578=CARTESIAN_POINT('Ctrl Pts',(11.0580951286388,-1.14954238521319,3.89106755072681));
#7579=CARTESIAN_POINT('Ctrl Pts',(11.0098010083862,-1.10620312192356,3.91213177324836));
#7580=CARTESIAN_POINT('Ctrl Pts',(10.984325834894,-1.08782446907905,3.92702466368572));
#7581=CARTESIAN_POINT('Ctrl Pts',(10.9440376044531,-1.06313017986469,3.95639578484302));
#7582=CARTESIAN_POINT('Ctrl Pts',(10.9255714846137,-1.05346991878665,3.97182573634243));
#7583=CARTESIAN_POINT('Ctrl Pts',(10.9031534277139,-1.04305739521201,3.99819879372234));
#7584=CARTESIAN_POINT('Ctrl Pts',(10.8966075473006,-1.04024696261202,4.00748456076932));
#7585=CARTESIAN_POINT('Ctrl Pts',(10.8869421569513,-1.03623280243464,4.02744119259084));
#7586=CARTESIAN_POINT('Ctrl Pts',(10.8837797594949,-1.035,4.03808539531883));
#7587=CARTESIAN_POINT('Ctrl Pts',(10.8837797594949,-1.035,4.05));
#7588=CARTESIAN_POINT('',(13.,-1.2,4.215));
#7589=CARTESIAN_POINT('',(9.9,-1.2,4.215));
#7590=CARTESIAN_POINT('Origin',(13.,-1.2,4.05));
#7591=CARTESIAN_POINT('Origin',(9.9,1.2,6.45));
#7592=CARTESIAN_POINT('',(10.,1.2,6.615));
#7593=CARTESIAN_POINT('Origin',(10.,1.2,6.45));
#7594=CARTESIAN_POINT('',(10.3,1.2,6.615));
#7595=CARTESIAN_POINT('',(9.9,1.2,6.615));
#7596=CARTESIAN_POINT('',(10.2185698389174,1.365,6.45));
#7597=CARTESIAN_POINT('Ctrl Pts',(10.2185698389174,1.365,6.45));
#7598=CARTESIAN_POINT('Ctrl Pts',(10.2185698389174,1.365,6.42900759846042));
#7599=CARTESIAN_POINT('Ctrl Pts',(10.2197033363378,1.36073611264639,6.40669500858237));
#7600=CARTESIAN_POINT('Ctrl Pts',(10.2249675898062,1.34371971020651,6.36599964223317));
#7601=CARTESIAN_POINT('Ctrl Pts',(10.2291861979204,1.33097165226366,6.3476264144721));
#7602=CARTESIAN_POINT('Ctrl Pts',(10.2410876841917,1.30077258467692,6.31742734688536));
#7603=CARTESIAN_POINT('Ctrl Pts',(10.249906982231,1.28099344112303,6.30456138651949));
#7604=CARTESIAN_POINT('Ctrl Pts',(10.2723294055107,1.2399125795835,6.28838530514966));
#7605=CARTESIAN_POINT('Ctrl Pts',(10.2859943020946,1.21867426387382,6.285));
#7606=CARTESIAN_POINT('Ctrl Pts',(10.3170531808664,1.17726242551144,6.285));
#7607=CARTESIAN_POINT('Ctrl Pts',(10.3373328915009,1.15455153425976,6.28988771813691));
#7608=CARTESIAN_POINT('Ctrl Pts',(10.3802569440026,1.11447899483743,6.30721461318364));
#7609=CARTESIAN_POINT('Ctrl Pts',(10.4028942700183,1.09707700316755,6.31957775904089));
#7610=CARTESIAN_POINT('Ctrl Pts',(10.4475863157778,1.0674330397717,6.34922172243674));
#7611=CARTESIAN_POINT('Ctrl Pts',(10.4762824962743,1.05234965200392,6.37165968077989));
#7612=CARTESIAN_POINT('Ctrl Pts',(10.5008967482507,1.04131297855552,6.4041576160186));
#7613=CARTESIAN_POINT('Ctrl Pts',(10.5063054900173,1.03902296892558,6.41262650433697));
#7614=CARTESIAN_POINT('Ctrl Pts',(10.5140205633862,1.0358566636217,6.43083371614971));
#7615=CARTESIAN_POINT('Ctrl Pts',(10.5162202405051,1.035,6.44062045354281));
#7616=CARTESIAN_POINT('Ctrl Pts',(10.5162202405051,1.035,6.46191460468117));
#7617=CARTESIAN_POINT('Ctrl Pts',(10.5130578430487,1.03623280243464,6.47255880740916));
#7618=CARTESIAN_POINT('Ctrl Pts',(10.5033924526994,1.04024696261203,6.49251543923068));
#7619=CARTESIAN_POINT('Ctrl Pts',(10.4968465722861,1.04305739521201,6.50180120627766));
#7620=CARTESIAN_POINT('Ctrl Pts',(10.4744285153863,1.05346991878665,6.52817426365758));
#7621=CARTESIAN_POINT('Ctrl Pts',(10.4559623955469,1.06313017986469,6.54360421515698));
#7622=CARTESIAN_POINT('Ctrl Pts',(10.415674165106,1.08782446907905,6.57297533631428));
#7623=CARTESIAN_POINT('Ctrl Pts',(10.3901989916138,1.10620312192356,6.58786822675164));
#7624=CARTESIAN_POINT('Ctrl Pts',(10.3419048713612,1.14954238521319,6.60893244927319));
#7625=CARTESIAN_POINT('Ctrl Pts',(10.319085409969,1.17455278670802,6.615));
#7626=CARTESIAN_POINT('Ctrl Pts',(10.3,1.2,6.615));
#7627=CARTESIAN_POINT('Ctrl Pts',(10.3,1.2,6.615));
#7628=CARTESIAN_POINT('Ctrl Pts',(10.2856850788648,1.21908656151361,6.615));
#7629=CARTESIAN_POINT('Ctrl Pts',(10.2717677906972,1.24080126498159,6.6114609819031));
#7630=CARTESIAN_POINT('Ctrl Pts',(10.2490773513426,1.28266254990227,6.59457281756084));
#7631=CARTESIAN_POINT('Ctrl Pts',(10.2402354326321,1.30274117773169,6.58114784976684));
#7632=CARTESIAN_POINT('Ctrl Pts',(10.2286736827823,1.33246344039378,6.55034605204221));
#7633=CARTESIAN_POINT('Ctrl Pts',(10.2246631762912,1.34467012765305,6.53222215412229));
#7634=CARTESIAN_POINT('Ctrl Pts',(10.2196511820674,1.360940751691,6.49228483534644));
#7635=CARTESIAN_POINT('Ctrl Pts',(10.2185698389174,1.365,6.47047956643719));
#7636=CARTESIAN_POINT('Ctrl Pts',(10.2185698389174,1.365,6.45));
#7637=CARTESIAN_POINT('Origin',(9.9,1.2,6.45));
#7638=CARTESIAN_POINT('',(11.1814301610826,1.365,6.45));
#7639=CARTESIAN_POINT('',(11.1,1.2,6.615));
#7640=CARTESIAN_POINT('Ctrl Pts',(11.1814301610826,1.365,6.45));
#7641=CARTESIAN_POINT('Ctrl Pts',(11.1814301610826,1.365,6.47047956643719));
#7642=CARTESIAN_POINT('Ctrl Pts',(11.1803488179326,1.360940751691,6.49228483534644));
#7643=CARTESIAN_POINT('Ctrl Pts',(11.1753368237088,1.34467012765305,6.53222215412229));
#7644=CARTESIAN_POINT('Ctrl Pts',(11.1713263172177,1.33246344039378,6.55034605204221));
#7645=CARTESIAN_POINT('Ctrl Pts',(11.1597645673678,1.30274117773169,6.58114784976684));
#7646=CARTESIAN_POINT('Ctrl Pts',(11.1509226486574,1.28266254990227,6.59457281756084));
#7647=CARTESIAN_POINT('Ctrl Pts',(11.1282322093028,1.24080126498159,6.6114609819031));
#7648=CARTESIAN_POINT('Ctrl Pts',(11.1143149211352,1.21908656151361,6.615));
#7649=CARTESIAN_POINT('Ctrl Pts',(11.1,1.2,6.615));
#7650=CARTESIAN_POINT('Ctrl Pts',(11.1,1.2,6.615));
#7651=CARTESIAN_POINT('Ctrl Pts',(11.080914590031,1.17455278670803,6.615));
#7652=CARTESIAN_POINT('Ctrl Pts',(11.0580951286388,1.14954238521319,6.60893244927319));
#7653=CARTESIAN_POINT('Ctrl Pts',(11.0098010083862,1.10620312192356,6.58786822675164));
#7654=CARTESIAN_POINT('Ctrl Pts',(10.984325834894,1.08782446907905,6.57297533631428));
#7655=CARTESIAN_POINT('Ctrl Pts',(10.9440376044531,1.06313017986469,6.54360421515698));
#7656=CARTESIAN_POINT('Ctrl Pts',(10.9255714846137,1.05346991878665,6.52817426365758));
#7657=CARTESIAN_POINT('Ctrl Pts',(10.9031534277139,1.04305739521201,6.50180120627766));
#7658=CARTESIAN_POINT('Ctrl Pts',(10.8966075473006,1.04024696261203,6.49251543923068));
#7659=CARTESIAN_POINT('Ctrl Pts',(10.8869421569513,1.03623280243464,6.47255880740916));
#7660=CARTESIAN_POINT('Ctrl Pts',(10.8837797594949,1.035,6.46191460468117));
#7661=CARTESIAN_POINT('Ctrl Pts',(10.8837797594949,1.035,6.44062045354281));
#7662=CARTESIAN_POINT('Ctrl Pts',(10.8859794366138,1.0358566636217,6.43083371614971));
#7663=CARTESIAN_POINT('Ctrl Pts',(10.8936945099827,1.03902296892558,6.41262650433697));
#7664=CARTESIAN_POINT('Ctrl Pts',(10.8991032517493,1.04131297855552,6.4041576160186));
#7665=CARTESIAN_POINT('Ctrl Pts',(10.9237175037257,1.05234965200392,6.37165968077989));
#7666=CARTESIAN_POINT('Ctrl Pts',(10.9524136842222,1.0674330397717,6.34922172243674));
#7667=CARTESIAN_POINT('Ctrl Pts',(10.9971057299817,1.09707700316755,6.31957775904089));
#7668=CARTESIAN_POINT('Ctrl Pts',(11.0197430559974,1.11447899483743,6.30721461318364));
#7669=CARTESIAN_POINT('Ctrl Pts',(11.0626671084991,1.15455153425976,6.28988771813691));
#7670=CARTESIAN_POINT('Ctrl Pts',(11.0829468191336,1.17726242551144,6.285));
#7671=CARTESIAN_POINT('Ctrl Pts',(11.1140056979054,1.21867426387382,6.285));
#7672=CARTESIAN_POINT('Ctrl Pts',(11.1276705944893,1.2399125795835,6.28838530514966));
#7673=CARTESIAN_POINT('Ctrl Pts',(11.150093017769,1.28099344112303,6.30456138651949));
#7674=CARTESIAN_POINT('Ctrl Pts',(11.1589123158083,1.30077258467692,6.31742734688536));
#7675=CARTESIAN_POINT('Ctrl Pts',(11.1708138020796,1.33097165226366,6.3476264144721));
#7676=CARTESIAN_POINT('Ctrl Pts',(11.1750324101937,1.34371971020651,6.36599964223317));
#7677=CARTESIAN_POINT('Ctrl Pts',(11.1802966636622,1.36073611264639,6.40669500858237));
#7678=CARTESIAN_POINT('Ctrl Pts',(11.1814301610826,1.365,6.42900759846042));
#7679=CARTESIAN_POINT('Ctrl Pts',(11.1814301610826,1.365,6.45));
#7680=CARTESIAN_POINT('',(13.,1.2,6.615));
#7681=CARTESIAN_POINT('',(9.9,1.2,6.615));
#7682=CARTESIAN_POINT('Origin',(13.,1.2,6.45));
#7683=CARTESIAN_POINT('Origin',(10.7,1.5,2.));
#7684=CARTESIAN_POINT('',(10.2,1.5,2.));
#7685=CARTESIAN_POINT('Origin',(10.7,1.5,2.));
#7686=CARTESIAN_POINT('',(10.2,1.5,2.));
#7687=CARTESIAN_POINT('',(10.917944947177,1.05,5.25));
#7688=CARTESIAN_POINT('Ctrl Pts',(10.917944947177,1.05,5.25));
#7689=CARTESIAN_POINT('Ctrl Pts',(10.917944947177,1.05,5.19751752176563));
#7690=CARTESIAN_POINT('Ctrl Pts',(10.9096209325494,1.04560657967159,5.14124876244566));
#7691=CARTESIAN_POINT('Ctrl Pts',(10.8813992178595,1.0339550375075,5.06535990747913));
#7692=CARTESIAN_POINT('Ctrl Pts',(10.8694149146398,1.02931935924876,5.04147273982077));
#7693=CARTESIAN_POINT('Ctrl Pts',(10.839847070119,1.01970376154596,4.99863134755478));
#7694=CARTESIAN_POINT('Ctrl Pts',(10.8223106862062,1.01472209320273,4.9796449878867));
#7695=CARTESIAN_POINT('Ctrl Pts',(10.7875957538804,1.00753000589576,4.954205579358));
#7696=CARTESIAN_POINT('Ctrl Pts',(10.7711257791067,1.0047701664708,4.9450775807219));
#7697=CARTESIAN_POINT('Ctrl Pts',(10.7360319592806,1.0009878010724,4.9328814434269));
#7698=CARTESIAN_POINT('Ctrl Pts',(10.7173937944281,1.,4.92984378812836));
#7699=CARTESIAN_POINT('Ctrl Pts',(10.6826062055719,1.,4.92984378812836));
#7700=CARTESIAN_POINT('Ctrl Pts',(10.6639680407194,1.0009878010724,4.9328814434269));
#7701=CARTESIAN_POINT('Ctrl Pts',(10.6288742208933,1.0047701664708,4.9450775807219));
#7702=CARTESIAN_POINT('Ctrl Pts',(10.6124042461196,1.00753000589576,4.954205579358));
#7703=CARTESIAN_POINT('Ctrl Pts',(10.5776893137938,1.01472209320273,4.9796449878867));
#7704=CARTESIAN_POINT('Ctrl Pts',(10.560152929881,1.01970376154596,4.99863134755478));
#7705=CARTESIAN_POINT('Ctrl Pts',(10.5305850853602,1.02931935924876,5.04147273982077));
#7706=CARTESIAN_POINT('Ctrl Pts',(10.5186007821405,1.0339550375075,5.06535990747913));
#7707=CARTESIAN_POINT('Ctrl Pts',(10.4903790674506,1.04560657967159,5.14124876244566));
#7708=CARTESIAN_POINT('Ctrl Pts',(10.482055052823,1.05,5.19751752176563));
#7709=CARTESIAN_POINT('Ctrl Pts',(10.482055052823,1.05,5.30248247823437));
#7710=CARTESIAN_POINT('Ctrl Pts',(10.4903790674506,1.04560657967159,5.35875123755434));
#7711=CARTESIAN_POINT('Ctrl Pts',(10.5186007821405,1.0339550375075,5.43464009252087));
#7712=CARTESIAN_POINT('Ctrl Pts',(10.5305850853602,1.02931935924876,5.45852726017924));
#7713=CARTESIAN_POINT('Ctrl Pts',(10.560152929881,1.01970376154596,5.50136865244522));
#7714=CARTESIAN_POINT('Ctrl Pts',(10.5776893137938,1.01472209320273,5.5203550121133));
#7715=CARTESIAN_POINT('Ctrl Pts',(10.6124042461196,1.00753000589576,5.545794420642));
#7716=CARTESIAN_POINT('Ctrl Pts',(10.6288742208933,1.0047701664708,5.5549224192781));
#7717=CARTESIAN_POINT('Ctrl Pts',(10.6639680407194,1.0009878010724,5.5671185565731));
#7718=CARTESIAN_POINT('Ctrl Pts',(10.6826062055719,1.,5.57015621187164));
#7719=CARTESIAN_POINT('Ctrl Pts',(10.7173937944281,1.,5.57015621187164));
#7720=CARTESIAN_POINT('Ctrl Pts',(10.7360319592806,1.0009878010724,5.5671185565731));
#7721=CARTESIAN_POINT('Ctrl Pts',(10.7711257791067,1.0047701664708,5.5549224192781));
#7722=CARTESIAN_POINT('Ctrl Pts',(10.7875957538804,1.00753000589576,5.545794420642));
#7723=CARTESIAN_POINT('Ctrl Pts',(10.8223106862062,1.01472209320273,5.5203550121133));
#7724=CARTESIAN_POINT('Ctrl Pts',(10.839847070119,1.01970376154596,5.50136865244522));
#7725=CARTESIAN_POINT('Ctrl Pts',(10.8694149146398,1.02931935924876,5.45852726017924));
#7726=CARTESIAN_POINT('Ctrl Pts',(10.8813992178595,1.0339550375075,5.43464009252087));
#7727=CARTESIAN_POINT('Ctrl Pts',(10.9096209325494,1.04560657967159,5.35875123755434));
#7728=CARTESIAN_POINT('Ctrl Pts',(10.917944947177,1.05,5.30248247823437));
#7729=CARTESIAN_POINT('Ctrl Pts',(10.917944947177,1.05,5.25));
#7730=CARTESIAN_POINT('Origin',(10.7,1.5,2.));
#7731=CARTESIAN_POINT('',(10.425,1.5,2.));
#7732=CARTESIAN_POINT('Origin',(10.7,1.5,2.));
#7733=CARTESIAN_POINT('Origin',(10.7,1.5,0.9));
#7734=CARTESIAN_POINT('',(10.425,1.5,1.));
#7735=CARTESIAN_POINT('Origin',(10.7,1.5,1.));
#7736=CARTESIAN_POINT('',(10.425,1.5,0.9));
#7737=CARTESIAN_POINT('Origin',(10.7,-1.5,2.));
#7738=CARTESIAN_POINT('',(10.2,-1.5,2.));
#7739=CARTESIAN_POINT('Origin',(10.7,-1.5,2.));
#7740=CARTESIAN_POINT('',(10.2,-1.5,2.));
#7741=CARTESIAN_POINT('',(10.482055052823,-1.05,5.25));
#7742=CARTESIAN_POINT('Ctrl Pts',(10.482055052823,-1.05,5.25));
#7743=CARTESIAN_POINT('Ctrl Pts',(10.482055052823,-1.05,5.19751752176563));
#7744=CARTESIAN_POINT('Ctrl Pts',(10.4903790674506,-1.04560657967159,5.14124876244566));
#7745=CARTESIAN_POINT('Ctrl Pts',(10.5186007821405,-1.0339550375075,5.06535990747913));
#7746=CARTESIAN_POINT('Ctrl Pts',(10.5305850853602,-1.02931935924876,5.04147273982077));
#7747=CARTESIAN_POINT('Ctrl Pts',(10.560152929881,-1.01970376154596,4.99863134755478));
#7748=CARTESIAN_POINT('Ctrl Pts',(10.5776893137938,-1.01472209320273,4.9796449878867));
#7749=CARTESIAN_POINT('Ctrl Pts',(10.6124042461196,-1.00753000589576,4.954205579358));
#7750=CARTESIAN_POINT('Ctrl Pts',(10.6288742208933,-1.0047701664708,4.9450775807219));
#7751=CARTESIAN_POINT('Ctrl Pts',(10.6639680407194,-1.0009878010724,4.9328814434269));
#7752=CARTESIAN_POINT('Ctrl Pts',(10.6826062055719,-1.,4.92984378812836));
#7753=CARTESIAN_POINT('Ctrl Pts',(10.7173937944281,-1.,4.92984378812836));
#7754=CARTESIAN_POINT('Ctrl Pts',(10.7360319592806,-1.0009878010724,4.9328814434269));
#7755=CARTESIAN_POINT('Ctrl Pts',(10.7711257791067,-1.0047701664708,4.9450775807219));
#7756=CARTESIAN_POINT('Ctrl Pts',(10.7875957538804,-1.00753000589576,4.954205579358));
#7757=CARTESIAN_POINT('Ctrl Pts',(10.8223106862062,-1.01472209320273,4.9796449878867));
#7758=CARTESIAN_POINT('Ctrl Pts',(10.839847070119,-1.01970376154596,4.99863134755478));
#7759=CARTESIAN_POINT('Ctrl Pts',(10.8694149146398,-1.02931935924876,5.04147273982077));
#7760=CARTESIAN_POINT('Ctrl Pts',(10.8813992178595,-1.0339550375075,5.06535990747913));
#7761=CARTESIAN_POINT('Ctrl Pts',(10.9096209325494,-1.04560657967159,5.14124876244566));
#7762=CARTESIAN_POINT('Ctrl Pts',(10.917944947177,-1.05,5.19751752176563));
#7763=CARTESIAN_POINT('Ctrl Pts',(10.917944947177,-1.05,5.30248247823437));
#7764=CARTESIAN_POINT('Ctrl Pts',(10.9096209325494,-1.04560657967159,5.35875123755434));
#7765=CARTESIAN_POINT('Ctrl Pts',(10.8813992178595,-1.0339550375075,5.43464009252087));
#7766=CARTESIAN_POINT('Ctrl Pts',(10.8694149146398,-1.02931935924876,5.45852726017923));
#7767=CARTESIAN_POINT('Ctrl Pts',(10.839847070119,-1.01970376154596,5.50136865244522));
#7768=CARTESIAN_POINT('Ctrl Pts',(10.8223106862062,-1.01472209320273,5.5203550121133));
#7769=CARTESIAN_POINT('Ctrl Pts',(10.7875957538804,-1.00753000589576,5.545794420642));
#7770=CARTESIAN_POINT('Ctrl Pts',(10.7711257791067,-1.0047701664708,5.5549224192781));
#7771=CARTESIAN_POINT('Ctrl Pts',(10.7360319592806,-1.0009878010724,5.5671185565731));
#7772=CARTESIAN_POINT('Ctrl Pts',(10.7173937944281,-1.,5.57015621187164));
#7773=CARTESIAN_POINT('Ctrl Pts',(10.6826062055719,-1.,5.57015621187164));
#7774=CARTESIAN_POINT('Ctrl Pts',(10.6639680407194,-1.0009878010724,5.5671185565731));
#7775=CARTESIAN_POINT('Ctrl Pts',(10.6288742208933,-1.0047701664708,5.5549224192781));
#7776=CARTESIAN_POINT('Ctrl Pts',(10.6124042461196,-1.00753000589576,5.545794420642));
#7777=CARTESIAN_POINT('Ctrl Pts',(10.5776893137938,-1.01472209320273,5.5203550121133));
#7778=CARTESIAN_POINT('Ctrl Pts',(10.560152929881,-1.01970376154596,5.50136865244522));
#7779=CARTESIAN_POINT('Ctrl Pts',(10.5305850853602,-1.02931935924876,5.45852726017923));
#7780=CARTESIAN_POINT('Ctrl Pts',(10.5186007821405,-1.0339550375075,5.43464009252087));
#7781=CARTESIAN_POINT('Ctrl Pts',(10.4903790674506,-1.04560657967159,5.35875123755434));
#7782=CARTESIAN_POINT('Ctrl Pts',(10.482055052823,-1.05,5.30248247823437));
#7783=CARTESIAN_POINT('Ctrl Pts',(10.482055052823,-1.05,5.25));
#7784=CARTESIAN_POINT('Origin',(10.7,-1.5,2.));
#7785=CARTESIAN_POINT('',(10.425,-1.5,2.));
#7786=CARTESIAN_POINT('Origin',(10.7,-1.5,2.));
#7787=CARTESIAN_POINT('Origin',(10.7,-1.5,0.9));
#7788=CARTESIAN_POINT('',(10.425,-1.5,1.));
#7789=CARTESIAN_POINT('Origin',(10.7,-1.5,1.));
#7790=CARTESIAN_POINT('',(10.425,-1.5,0.9));
#7791=CARTESIAN_POINT('Origin',(9.9,0.,5.25));
#7792=CARTESIAN_POINT('',(10.,-1.28587913910472E-16,6.3));
#7793=CARTESIAN_POINT('Origin',(10.,0.,5.25));
#7794=CARTESIAN_POINT('',(13.,1.28587913910472E-16,6.3));
#7795=CARTESIAN_POINT('',(9.9,-1.28587913910472E-16,6.3));
#7796=CARTESIAN_POINT('Origin',(13.,0.,5.25));
#7797=CARTESIAN_POINT('Origin',(13.,-2.,1.));
#7798=CARTESIAN_POINT('',(13.,-2.,1.));
#7799=CARTESIAN_POINT('Origin',(10.,2.,1.));
#7800=CARTESIAN_POINT('',(10.,2.,1.));
#7801=CARTESIAN_POINT('Origin',(11.5,0.,1.));
#7802=CARTESIAN_POINT('',(0.,0.,0.));
#7803=CARTESIAN_POINT('Origin',(9.6,1.2,4.05));
#7804=CARTESIAN_POINT('',(9.7,1.26887332488551,3.83580040821884));
#7805=CARTESIAN_POINT('',(10.,1.26887332488551,3.83580040821884));
#7806=CARTESIAN_POINT('',(9.6,1.26887332488551,3.83580040821884));
#7807=CARTESIAN_POINT('',(9.7,1.41419959178116,3.98112667511449));
#7808=CARTESIAN_POINT('Origin',(9.7,1.2,4.05));
#7809=CARTESIAN_POINT('',(10.,1.41419959178116,3.98112667511449));
#7810=CARTESIAN_POINT('',(9.6,1.41419959178116,3.98112667511449));
#7811=CARTESIAN_POINT('Origin',(10.,1.2,4.05));
#7812=CARTESIAN_POINT('Origin',(9.6,-1.2,6.45));
#7813=CARTESIAN_POINT('',(9.7,-1.26887332488551,6.66419959178116));
#7814=CARTESIAN_POINT('',(10.,-1.26887332488551,6.66419959178116));
#7815=CARTESIAN_POINT('',(9.6,-1.26887332488551,6.66419959178116));
#7816=CARTESIAN_POINT('',(9.7,-1.41419959178116,6.51887332488551));
#7817=CARTESIAN_POINT('Origin',(9.7,-1.2,6.45));
#7818=CARTESIAN_POINT('',(10.,-1.41419959178116,6.51887332488551));
#7819=CARTESIAN_POINT('',(9.6,-1.41419959178116,6.51887332488551));
#7820=CARTESIAN_POINT('Origin',(10.,-1.2,6.45));
#7821=CARTESIAN_POINT('Origin',(9.6,-1.2,4.05));
#7822=CARTESIAN_POINT('',(9.7,-1.41419959178116,3.98112667511449));
#7823=CARTESIAN_POINT('',(10.,-1.41419959178116,3.98112667511449));
#7824=CARTESIAN_POINT('',(9.6,-1.41419959178116,3.98112667511449));
#7825=CARTESIAN_POINT('',(9.7,-1.26887332488551,3.83580040821884));
#7826=CARTESIAN_POINT('Origin',(9.7,-1.2,4.05));
#7827=CARTESIAN_POINT('',(10.,-1.26887332488551,3.83580040821884));
#7828=CARTESIAN_POINT('',(9.6,-1.26887332488551,3.83580040821884));
#7829=CARTESIAN_POINT('Origin',(10.,-1.2,4.05));
#7830=CARTESIAN_POINT('Origin',(9.6,1.2,6.45));
#7831=CARTESIAN_POINT('',(9.7,1.41419959178116,6.51887332488551));
#7832=CARTESIAN_POINT('',(10.,1.41419959178116,6.51887332488551));
#7833=CARTESIAN_POINT('',(9.6,1.41419959178116,6.51887332488551));
#7834=CARTESIAN_POINT('',(9.7,1.26887332488551,6.66419959178116));
#7835=CARTESIAN_POINT('Origin',(9.7,1.2,6.45));
#7836=CARTESIAN_POINT('',(10.,1.26887332488551,6.66419959178116));
#7837=CARTESIAN_POINT('',(9.6,1.26887332488551,6.66419959178116));
#7838=CARTESIAN_POINT('Origin',(10.,1.2,6.45));
#7839=CARTESIAN_POINT('Origin',(9.7,0.,5.25));
#7840=CARTESIAN_POINT('Origin',(9.7,0.,5.25));
#7841=CARTESIAN_POINT('Origin',(9.7,0.,5.25));
#7842=CARTESIAN_POINT('Origin',(9.7,0.,5.25));
#7843=CARTESIAN_POINT('Origin',(9.7,0.,5.25));
#7844=CARTESIAN_POINT('',(9.7,-7.59281015471359E-17,5.87));
#7845=CARTESIAN_POINT('Origin',(9.7,0.,5.25));
#7846=CARTESIAN_POINT('Origin',(9.7,0.,5.25));
#7847=CARTESIAN_POINT('Origin',(10.,0.,5.25));
#7848=CARTESIAN_POINT('Origin',(9.7,0.,5.25));
#7849=CARTESIAN_POINT('Origin',(10.,0.,5.25));
#7850=CARTESIAN_POINT('Origin',(9.7,0.,5.25));
#7851=CARTESIAN_POINT('Origin',(10.,0.,5.25));
#7852=CARTESIAN_POINT('Origin',(9.7,0.,5.25));
#7853=CARTESIAN_POINT('Origin',(10.,0.,5.25));
#7854=CARTESIAN_POINT('Origin',(9.7,0.,5.25));
#7855=CARTESIAN_POINT('',(10.,-7.59281015471359E-17,5.87));
#7856=CARTESIAN_POINT('Origin',(10.,0.,5.25));
#7857=CARTESIAN_POINT('',(9.7,-7.59281015471359E-17,5.87));
#7858=CARTESIAN_POINT('Origin',(10.,0.,5.25));
#7859=CARTESIAN_POINT('',(0.,0.,0.));
#7860=CARTESIAN_POINT('Origin',(12.9,1.2,4.05));
#7861=CARTESIAN_POINT('',(13.,1.26887332488551,3.83580040821884));
#7862=CARTESIAN_POINT('',(13.3,1.26887332488551,3.83580040821884));
#7863=CARTESIAN_POINT('',(12.9,1.26887332488551,3.83580040821884));
#7864=CARTESIAN_POINT('',(13.,1.41419959178116,3.98112667511449));
#7865=CARTESIAN_POINT('Origin',(13.,1.2,4.05));
#7866=CARTESIAN_POINT('',(13.3,1.41419959178116,3.98112667511449));
#7867=CARTESIAN_POINT('',(12.9,1.41419959178116,3.98112667511449));
#7868=CARTESIAN_POINT('Origin',(13.3,1.2,4.05));
#7869=CARTESIAN_POINT('Origin',(12.9,-1.2,6.45));
#7870=CARTESIAN_POINT('',(13.,-1.26887332488551,6.66419959178116));
#7871=CARTESIAN_POINT('',(13.3,-1.26887332488551,6.66419959178116));
#7872=CARTESIAN_POINT('',(12.9,-1.26887332488551,6.66419959178116));
#7873=CARTESIAN_POINT('',(13.,-1.41419959178116,6.51887332488551));
#7874=CARTESIAN_POINT('Origin',(13.,-1.2,6.45));
#7875=CARTESIAN_POINT('',(13.3,-1.41419959178116,6.51887332488551));
#7876=CARTESIAN_POINT('',(12.9,-1.41419959178116,6.51887332488551));
#7877=CARTESIAN_POINT('Origin',(13.3,-1.2,6.45));
#7878=CARTESIAN_POINT('Origin',(12.9,-1.2,4.05));
#7879=CARTESIAN_POINT('',(13.,-1.41419959178116,3.98112667511449));
#7880=CARTESIAN_POINT('',(13.3,-1.41419959178116,3.98112667511449));
#7881=CARTESIAN_POINT('',(12.9,-1.41419959178116,3.98112667511449));
#7882=CARTESIAN_POINT('',(13.,-1.26887332488551,3.83580040821884));
#7883=CARTESIAN_POINT('Origin',(13.,-1.2,4.05));
#7884=CARTESIAN_POINT('',(13.3,-1.26887332488551,3.83580040821884));
#7885=CARTESIAN_POINT('',(12.9,-1.26887332488551,3.83580040821884));
#7886=CARTESIAN_POINT('Origin',(13.3,-1.2,4.05));
#7887=CARTESIAN_POINT('Origin',(12.9,1.2,6.45));
#7888=CARTESIAN_POINT('',(13.,1.41419959178116,6.51887332488551));
#7889=CARTESIAN_POINT('',(13.3,1.41419959178116,6.51887332488551));
#7890=CARTESIAN_POINT('',(12.9,1.41419959178116,6.51887332488551));
#7891=CARTESIAN_POINT('',(13.,1.26887332488551,6.66419959178116));
#7892=CARTESIAN_POINT('Origin',(13.,1.2,6.45));
#7893=CARTESIAN_POINT('',(13.3,1.26887332488551,6.66419959178116));
#7894=CARTESIAN_POINT('',(12.9,1.26887332488551,6.66419959178116));
#7895=CARTESIAN_POINT('Origin',(13.3,1.2,6.45));
#7896=CARTESIAN_POINT('Origin',(13.,0.,5.25));
#7897=CARTESIAN_POINT('Origin',(13.,0.,5.25));
#7898=CARTESIAN_POINT('Origin',(13.,0.,5.25));
#7899=CARTESIAN_POINT('Origin',(13.,0.,5.25));
#7900=CARTESIAN_POINT('Origin',(13.,0.,5.25));
#7901=CARTESIAN_POINT('',(13.,-7.59281015471359E-17,5.87));
#7902=CARTESIAN_POINT('Origin',(13.,0.,5.25));
#7903=CARTESIAN_POINT('Origin',(13.,0.,5.25));
#7904=CARTESIAN_POINT('Origin',(13.3,0.,5.25));
#7905=CARTESIAN_POINT('Origin',(13.,0.,5.25));
#7906=CARTESIAN_POINT('Origin',(13.3,0.,5.25));
#7907=CARTESIAN_POINT('Origin',(13.,0.,5.25));
#7908=CARTESIAN_POINT('Origin',(13.3,0.,5.25));
#7909=CARTESIAN_POINT('Origin',(13.,0.,5.25));
#7910=CARTESIAN_POINT('Origin',(13.3,0.,5.25));
#7911=CARTESIAN_POINT('Origin',(13.,0.,5.25));
#7912=CARTESIAN_POINT('',(13.3,-7.59281015471359E-17,5.87));
#7913=CARTESIAN_POINT('Origin',(13.3,0.,5.25));
#7914=CARTESIAN_POINT('',(13.,-7.59281015471359E-17,5.87));
#7915=CARTESIAN_POINT('Origin',(13.3,0.,5.25));
#7916=CARTESIAN_POINT('',(0.,0.,0.));
#7917=CARTESIAN_POINT('Ctrl Pts',(6.55994469204049,0.719709328495781,5.24703997894806));
#7918=CARTESIAN_POINT('Ctrl Pts',(6.56494552765653,0.719691145920131,5.38210508200347));
#7919=CARTESIAN_POINT('Ctrl Pts',(6.57494016333875,0.642089168505731,5.65058609468785));
#7920=CARTESIAN_POINT('Ctrl Pts',(6.58989438616266,0.32941528595114,5.9296313569664));
#7921=CARTESIAN_POINT('Ctrl Pts',(6.60481477071411,-0.0827797453005289,
5.99886361370576));
#7922=CARTESIAN_POINT('Ctrl Pts',(6.61969980345594,-0.467619845512657,5.83844773036597));
#7923=CARTESIAN_POINT('Ctrl Pts',(6.63454965842308,-0.707639327219362,5.49857002500469));
#7924=CARTESIAN_POINT('Ctrl Pts',(6.64936061260475,-0.729495436544756,5.0840660001111));
#7925=CARTESIAN_POINT('Ctrl Pts',(6.66414030226907,-0.527844751315962,4.72224444577032));
#7926=CARTESIAN_POINT('Ctrl Pts',(6.67641810037933,-0.225796647591973,4.55722222010489));
#7927=CARTESIAN_POINT('Ctrl Pts',(6.68623494447203,0.0403746271135037,4.5362580751361));
#7928=CARTESIAN_POINT('Ctrl Pts',(6.69357256905876,0.236291461979514,4.57606849800983));
#7929=CARTESIAN_POINT('Ctrl Pts',(6.70093718034598,0.413303779793928,4.66864974641035));
#7930=CARTESIAN_POINT('Ctrl Pts',(6.70820868996388,0.557592736564421,4.80642809587619));
#7931=CARTESIAN_POINT('Ctrl Pts',(6.71380490830661,0.632807795501951,4.93556873282767));
#7932=CARTESIAN_POINT('Ctrl Pts',(6.71731244248601,0.666836920456702,5.02812885948168));
#7933=CARTESIAN_POINT('Ctrl Pts',(6.71917582310349,0.680406120596861,5.07513188532028));
#7934=CARTESIAN_POINT('Ctrl Pts',(6.72133213271133,0.6909093875254,5.1233938812218));
#7935=CARTESIAN_POINT('Ctrl Pts',(6.72306773259333,0.700241175081311,5.19054637990825));
#7936=CARTESIAN_POINT('Ctrl Pts',(6.72619261442483,0.703178325652587,5.2668476785023));
#7937=CARTESIAN_POINT('Ctrl Pts',(6.7381664251681,0.689514001675121,5.39852659753196));
#7938=CARTESIAN_POINT('Ctrl Pts',(6.75463925550615,0.618247264838858,5.61826960075177));
#7939=CARTESIAN_POINT('Ctrl Pts',(6.77590827674278,0.436470460186145,5.81941560675087));
#7940=CARTESIAN_POINT('Ctrl Pts',(6.79564326301645,0.196280809931693,5.9247163591309));
#7941=CARTESIAN_POINT('Ctrl Pts',(6.81582644522033,-0.0629302930494358,
5.96025522192144));
#7942=CARTESIAN_POINT('Ctrl Pts',(6.84069654900574,-0.38497400844017,5.86555713916006));
#7943=CARTESIAN_POINT('Ctrl Pts',(6.86947638412051,-0.640427331596973,5.57601421543896));
#7944=CARTESIAN_POINT('Ctrl Pts',(6.89697365083529,-0.710923798883682,5.21615884811777));
#7945=CARTESIAN_POINT('Ctrl Pts',(6.92329898795441,-0.605777386429107,4.88177837844538));
#7946=CARTESIAN_POINT('Ctrl Pts',(6.94951107797999,-0.354456178032768,4.63917675459059));
#7947=CARTESIAN_POINT('Ctrl Pts',(6.97563701108018,-0.0190898795841548,
4.54673256040166));
#7948=CARTESIAN_POINT('Ctrl Pts',(7.00166306815893,0.318420157020357,4.6254869521555));
#7949=CARTESIAN_POINT('Ctrl Pts',(7.02543388521809,0.554722542828515,4.83645416115326));
#7950=CARTESIAN_POINT('Ctrl Pts',(7.04697773806416,0.666084600719225,5.09617679024369));
#7951=CARTESIAN_POINT('Ctrl Pts',(7.07276315353201,0.678427725557665,5.43526847721852));
#7952=CARTESIAN_POINT('Ctrl Pts',(7.10058962059944,0.484472501752673,5.76690932949108));
#7953=CARTESIAN_POINT('Ctrl Pts',(7.13043692169364,0.120638399689201,5.92825455906627));
#7954=CARTESIAN_POINT('Ctrl Pts',(7.1559402685194,-0.217537459809761,5.90145833585114));
#7955=CARTESIAN_POINT('Ctrl Pts',(7.17606991375773,-0.442156866353605,5.75500273582888));
#7956=CARTESIAN_POINT('Ctrl Pts',(7.1908732639631,-0.55830610816236,5.60220615030058));
#7957=CARTESIAN_POINT('Ctrl Pts',(7.20354845498638,-0.631705810891337,5.45532626907927));
#7958=CARTESIAN_POINT('Ctrl Pts',(7.22569553162755,-0.685810607871027,5.1691057765553));
#7959=CARTESIAN_POINT('Ctrl Pts',(7.25723947880328,-0.525122526582691,4.7636055764722));
#7960=CARTESIAN_POINT('Ctrl Pts',(7.29495362238925,-0.053457135933399,4.53870854204931));
#7961=CARTESIAN_POINT('Ctrl Pts',(7.33254246780218,0.443142598581714,4.69413693222259));
#7962=CARTESIAN_POINT('Ctrl Pts',(7.37001978026861,0.701091243696442,5.14423427781829));
#7963=CARTESIAN_POINT('Ctrl Pts',(7.40739968824424,0.584157721738047,5.64880921553006));
#7964=CARTESIAN_POINT('Ctrl Pts',(7.43848048896546,0.228011772623945,5.88938664283398));
#7965=CARTESIAN_POINT('Ctrl Pts',(7.46331103237168,-0.0982454758707846,
5.89962806423389));
#7966=CARTESIAN_POINT('Ctrl Pts',(7.48398628613683,-0.354294590444537,5.80983193950292));
#7967=CARTESIAN_POINT('Ctrl Pts',(7.50671008387199,-0.570451156260486,5.59791253961241));
#7968=CARTESIAN_POINT('Ctrl Pts',(7.53148051029953,-0.667000675030891,5.28247942808214));
#7969=CARTESIAN_POINT('Ctrl Pts',(7.55211030997723,-0.61172699107091,5.01340213779963));
#7970=CARTESIAN_POINT('Ctrl Pts',(7.56860908294787,-0.494743373007304,4.8335093105102));
#7971=CARTESIAN_POINT('Ctrl Pts',(7.58510523358743,-0.337168872759663,4.68756299395369));
#7972=CARTESIAN_POINT('Ctrl Pts',(7.60572192687897,-0.0819019612031444,
4.58805237352457));
#7973=CARTESIAN_POINT('Ctrl Pts',(7.63458408889819,0.300170619986696,4.63555033917682));
#7974=CARTESIAN_POINT('Ctrl Pts',(7.66138943476793,0.571053603076512,4.88796924826266));
#7975=CARTESIAN_POINT('Ctrl Pts',(7.68614446458683,0.653366892065435,5.20295921197447));
#7976=CARTESIAN_POINT('Ctrl Pts',(7.71090979818012,0.617991353788974,5.52603673989692));
#7977=CARTESIAN_POINT('Ctrl Pts',(7.74189055099461,0.350623503322525,5.86154592695952));
#7978=CARTESIAN_POINT('Ctrl Pts',(7.77601859800523,-0.116495965826188,5.93082813098408));
#7979=CARTESIAN_POINT('Ctrl Pts',(7.80709414997369,-0.481412412605556,5.72789933690448));
#7980=CARTESIAN_POINT('Ctrl Pts',(7.83510698559819,-0.663163478596285,5.39892523906655));
#7981=CARTESIAN_POINT('Ctrl Pts',(7.85615485977222,-0.647079306054213,5.11675578479515));
#7982=CARTESIAN_POINT('Ctrl Pts',(7.87020459706828,-0.574886104874813,4.94990033899215));
#7983=CARTESIAN_POINT('Ctrl Pts',(7.87723312367712,-0.527583060020924,4.87226677612988));
#7984=CARTESIAN_POINT('Ctrl Pts',(7.88426540124521,-0.469793796464868,4.80191051673322));
#7985=CARTESIAN_POINT('Ctrl Pts',(7.89521047892777,-0.365529336701908,4.7063343213378));
#7986=CARTESIAN_POINT('Ctrl Pts',(7.91634048666751,-0.120063962380262,4.57508935662309));
#7987=CARTESIAN_POINT('Ctrl Pts',(7.94458071734118,0.268642859242054,4.60441791433467));
#7988=CARTESIAN_POINT('Ctrl Pts',(7.97605533596052,0.584027938453731,4.88737223927164));
#7989=CARTESIAN_POINT('Ctrl Pts',(8.00446254702578,0.689638060716412,5.2531749302134));
#7990=CARTESIAN_POINT('Ctrl Pts',(8.03295521872146,0.583958260807566,5.62109535966095));
#7991=CARTESIAN_POINT('Ctrl Pts',(8.06153860386915,0.297951770638925,5.87686527268886));
#7992=CARTESIAN_POINT('Ctrl Pts',(8.09021776831132,-0.0816004700383042,
5.94171985993802));
#7993=CARTESIAN_POINT('Ctrl Pts',(8.11899761019108,-0.438736741574054,5.7941606881638));
#7994=CARTESIAN_POINT('Ctrl Pts',(8.14788283876726,-0.66350439566471,5.47812772009615));
#7995=CARTESIAN_POINT('Ctrl Pts',(8.17687795851733,-0.6858207744463,5.08946678694388));
#7996=CARTESIAN_POINT('Ctrl Pts',(8.20598727446933,-0.497249207778955,4.74714184053921));
#7997=CARTESIAN_POINT('Ctrl Pts',(8.23521486961617,-0.154093127286878,4.55679071733693));
#7998=CARTESIAN_POINT('Ctrl Pts',(8.26456461818433,0.239380388009074,4.57821827016813));
#7999=CARTESIAN_POINT('Ctrl Pts',(8.29404014876887,0.562549974717286,4.80663318942082));
#8000=CARTESIAN_POINT('Ctrl Pts',(8.32364486518472,0.715391021033525,5.17354565176085));
#8001=CARTESIAN_POINT('Ctrl Pts',(8.35338192623768,0.649330974858417,5.56731319891309));
#8002=CARTESIAN_POINT('Ctrl Pts',(8.38325424070601,0.382790348017333,5.86693311075399));
#8003=CARTESIAN_POINT('Ctrl Pts',(8.41326446409716,-0.00419505000370753,
5.97947359705855));
#8004=CARTESIAN_POINT('Ctrl Pts',(8.43838990507217,-0.328427739096548,5.88675138216907));
#8005=CARTESIAN_POINT('Ctrl Pts',(8.45856147729175,-0.529480619639225,5.71722997945441));
#8006=CARTESIAN_POINT('Ctrl Pts',(8.47765754585014,-0.668434606896997,5.5107649981822));
#8007=CARTESIAN_POINT('Ctrl Pts',(8.50076123794206,-0.730336170493974,5.20937619755011));
#8008=CARTESIAN_POINT('Ctrl Pts',(8.52792461605616,-0.624513035959022,4.86362366838459));
#8009=CARTESIAN_POINT('Ctrl Pts',(8.5529308052989,-0.386883838373545,4.6302289824672));
#8010=CARTESIAN_POINT('Ctrl Pts',(8.57574894485481,-0.104298108040022,4.53121501380808));
#8011=CARTESIAN_POINT('Ctrl Pts',(8.6032187287894,0.256675810750089,4.54226136093568));
#8012=CARTESIAN_POINT('Ctrl Pts',(8.63772155686955,0.652405168310869,4.80876975888547));
#8013=CARTESIAN_POINT('Ctrl Pts',(8.67939097890975,0.783030401351032,5.37140034010679));
#8014=CARTESIAN_POINT('Ctrl Pts',(8.72132656843746,0.49495090614558,5.87513455402037));
#8015=CARTESIAN_POINT('Ctrl Pts',(8.76352759225084,-0.0628635021467805,
6.05013777316939));
#8016=CARTESIAN_POINT('Ctrl Pts',(8.79891493140875,-0.504716359285686,5.83905645697925));
#8017=CARTESIAN_POINT('Ctrl Pts',(8.82735545219243,-0.703159459402567,5.5227896978014));
#8018=CARTESIAN_POINT('Ctrl Pts',(8.85588259535385,-0.776061781005718,5.15482469233793));
#8019=CARTESIAN_POINT('Ctrl Pts',(8.88692644387892,-0.621492770362474,4.75483748689365));
#8020=CARTESIAN_POINT('Ctrl Pts',(8.92052297991862,-0.245496738926199,4.51104937209089));
#8021=CARTESIAN_POINT('Ctrl Pts',(8.94943095663315,0.137693585331708,4.48033145317999));
#8022=CARTESIAN_POINT('Ctrl Pts',(8.97965767299615,0.505669735297425,4.64426980471776));
#8023=CARTESIAN_POINT('Ctrl Pts',(9.01121604967911,0.752482582266742,4.98850418901732));
#8024=CARTESIAN_POINT('Ctrl Pts',(9.04412144632782,0.779510405814253,5.42959222113123));
#8025=CARTESIAN_POINT('Ctrl Pts',(9.07715711994043,0.566889248726445,5.81885947968755));
#8026=CARTESIAN_POINT('Ctrl Pts',(9.11031735538565,0.178292209075846,6.0362617860296));
#8027=CARTESIAN_POINT('Ctrl Pts',(9.14360253722173,-0.268079437778697,6.01351727669282));
#8028=CARTESIAN_POINT('Ctrl Pts',(9.17699734546285,-0.635285771434068,5.75590592911153));
#8029=CARTESIAN_POINT('Ctrl Pts',(9.21051983173094,-0.809796215592389,5.34095865996421));
#8030=CARTESIAN_POINT('Ctrl Pts',(9.24411094986739,-0.736619369561702,4.89534022537719));
#8031=CARTESIAN_POINT('Ctrl Pts',(9.27788074499435,-0.436616793358521,4.55570108560577));
#8032=CARTESIAN_POINT('Ctrl Pts',(9.30594116368128,-0.0733420592947115,
4.44897069772665));
#8033=CARTESIAN_POINT('Ctrl Pts',(9.328680473888,0.218704827060702,4.48901682699427));
#8034=CARTESIAN_POINT('Ctrl Pts',(9.35089495840618,0.489065381509997,4.60762593183536));
#8035=CARTESIAN_POINT('Ctrl Pts',(9.37480209610635,0.693278005812641,4.83358316838714));
#8036=CARTESIAN_POINT('Ctrl Pts',(9.39327740184756,0.773205179450414,5.08031011736591));
#8037=CARTESIAN_POINT('Ctrl Pts',(9.40667901531909,0.788514168138214,5.22730031946394));
#8038=CARTESIAN_POINT('Ctrl Pts',(9.41035265957923,0.785191918284243,5.31605807341251));
#8039=CARTESIAN_POINT('Ctrl Pts',(9.41223809751033,0.774762970480976,5.39019446309586));
#8040=CARTESIAN_POINT('Ctrl Pts',(9.4146591021466,0.763068583364469,5.44423938068532));
#8041=CARTESIAN_POINT('Ctrl Pts',(9.4167523666832,0.747778571803171,5.49710428778674));
#8042=CARTESIAN_POINT('Ctrl Pts',(9.42068446598339,0.709658392601865,5.60083098220104));
#8043=CARTESIAN_POINT('Ctrl Pts',(9.42695148511213,0.625399217361514,5.74546397737963));
#8044=CARTESIAN_POINT('Ctrl Pts',(9.4350913459169,0.463897848898915,5.89967743034001));
#8045=CARTESIAN_POINT('Ctrl Pts',(9.44332988824765,0.265871334396363,6.00323600320908));
#8046=CARTESIAN_POINT('Ctrl Pts',(9.45153347644623,0.0468430344411857,6.04773546710682));
#8047=CARTESIAN_POINT('Ctrl Pts',(9.46250188685132,-0.250556076226033,6.02429177474909));
#8048=CARTESIAN_POINT('Ctrl Pts',(9.47620737800529,-0.587650060167328,5.84004639330421));
#8049=CARTESIAN_POINT('Ctrl Pts',(9.49268366719886,-0.81241635296479,5.43659555942134));
#8050=CARTESIAN_POINT('Ctrl Pts',(9.50917374900608,-0.787865415172378,4.9752477474741));
#8051=CARTESIAN_POINT('Ctrl Pts',(9.52568233488031,-0.521201295938573,4.59717415541696));
#8052=CARTESIAN_POINT('Ctrl Pts',(9.5422061736552,-0.0937383220535699,4.41946428983354));
#8053=CARTESIAN_POINT('Ctrl Pts',(9.55874735915243,0.363109547604185,4.49620059730279));
#8054=CARTESIAN_POINT('Ctrl Pts',(9.57529830568314,0.709172657538417,4.80516325810888));
#8055=CARTESIAN_POINT('Ctrl Pts',(9.58634758255215,0.794862864598598,5.10196837702893));
#8056=CARTESIAN_POINT('Ctrl Pts',(9.59186670251247,0.79488293160754,5.25103156499837));
#8057=CARTESIAN_POINT('Ctrl Pts',(6.5600317203433,0.743645114310226,5.24703997894806));
#8058=CARTESIAN_POINT('Ctrl Pts',(6.56519694359966,0.743626334036324,5.38654494671483));
#8059=CARTESIAN_POINT('Ctrl Pts',(6.57552575104629,0.663439491064011,5.66398423458453));
#8060=CARTESIAN_POINT('Ctrl Pts',(6.59097732705008,0.340362727022784,5.95229610571387));
#8061=CARTESIAN_POINT('Ctrl Pts',(6.60639588256248,-0.085564624808665,6.02384672671786));
#8062=CARTESIAN_POINT('Ctrl Pts',(6.62177750449655,-0.483232072698951,5.85808296752321));
#8063=CARTESIAN_POINT('Ctrl Pts',(6.63712358115281,-0.73125343445,5.50687494047551));
#8064=CARTESIAN_POINT('Ctrl Pts',(6.65243043600796,-0.753834594795398,5.07854546230159));
#8065=CARTESIAN_POINT('Ctrl Pts',(6.6677040836227,-0.545458428391592,4.70466776269486));
#8066=CARTESIAN_POINT('Ctrl Pts',(6.68039282388046,-0.23334272044992,4.53415317767454));
#8067=CARTESIAN_POINT('Ctrl Pts',(6.69053665092139,0.0416796042804993,4.51249422389647));
#8068=CARTESIAN_POINT('Ctrl Pts',(6.69811867522059,0.244107755344965,4.55362929691641));
#8069=CARTESIAN_POINT('Ctrl Pts',(6.70572848762197,0.426997624599347,4.64928698265267));
#8070=CARTESIAN_POINT('Ctrl Pts',(6.713241694215,0.576073511958108,4.79163606897931));
#8071=CARTESIAN_POINT('Ctrl Pts',(6.71902424219905,0.653781708136255,4.92505878976939));
#8072=CARTESIAN_POINT('Ctrl Pts',(6.72264773696813,0.688937202960286,5.0206791373597));
#8073=CARTESIAN_POINT('Ctrl Pts',(6.72457239960857,0.702948690130069,5.069221824819));
#8074=CARTESIAN_POINT('Ctrl Pts',(6.72679968927165,0.713804995118134,5.1190819534982));
#8075=CARTESIAN_POINT('Ctrl Pts',(6.7285973777106,0.723447631782051,5.18854189286989));
#8076=CARTESIAN_POINT('Ctrl Pts',(6.73181253270818,0.726479171259777,5.26711526304695));
#8077=CARTESIAN_POINT('Ctrl Pts',(6.74418104973988,0.712364538955456,5.40315993041796));
#8078=CARTESIAN_POINT('Ctrl Pts',(6.76119416892908,0.638762136278474,5.63009066315064));
#8079=CARTESIAN_POINT('Ctrl Pts',(6.78316216266072,0.451029028315658,5.83780909913891));
#8080=CARTESIAN_POINT('Ctrl Pts',(6.80353597647317,0.203074911136787,5.94650492858841));
#8081=CARTESIAN_POINT('Ctrl Pts',(6.8243697854844,-0.0644746999694365,5.98318447082224));
#8082=CARTESIAN_POINT('Ctrl Pts',(6.85003803144352,-0.396790077585058,5.885439852334));
#8083=CARTESIAN_POINT('Ctrl Pts',(6.8797274902126,-0.660254447903026,5.586770643378));
#8084=CARTESIAN_POINT('Ctrl Pts',(6.90808044479718,-0.732907685022115,5.21576889406585));
#8085=CARTESIAN_POINT('Ctrl Pts',(6.93521165231085,-0.624533500927869,4.87121325841169));
#8086=CARTESIAN_POINT('Ctrl Pts',(6.96221299448147,-0.365673416845925,4.62137630968268));
#8087=CARTESIAN_POINT('Ctrl Pts',(6.98910503562642,-0.0204912870103402,
4.52625933591179));
#8088=CARTESIAN_POINT('Ctrl Pts',(7.01587828254526,0.326664127736654,4.60729823930461));
#8089=CARTESIAN_POINT('Ctrl Pts',(7.04031755717951,0.569540378656345,4.82418452570712));
#8090=CARTESIAN_POINT('Ctrl Pts',(7.06244951669149,0.683917755846529,5.09097740656128));
#8091=CARTESIAN_POINT('Ctrl Pts',(7.08892444932795,0.696562702579088,5.43910230418443));
#8092=CARTESIAN_POINT('Ctrl Pts',(7.11747479399797,0.497535769821888,5.77923828692686));
#8093=CARTESIAN_POINT('Ctrl Pts',(7.14805659228038,0.12476158764217,5.9444858162509));
#8094=CARTESIAN_POINT('Ctrl Pts',(7.17416577049173,-0.221392458573116,5.91702498690739));
#8095=CARTESIAN_POINT('Ctrl Pts',(7.19475934143304,-0.451091723068877,5.76721176820514));
#8096=CARTESIAN_POINT('Ctrl Pts',(7.20988756684039,-0.569776469467092,5.6110768737848));
#8097=CARTESIAN_POINT('Ctrl Pts',(7.22283668157726,-0.644749444213715,5.46104198585997));
#8098=CARTESIAN_POINT('Ctrl Pts',(7.2454490573998,-0.699961029561219,5.16883668420344));
#8099=CARTESIAN_POINT('Ctrl Pts',(7.27762148574156,-0.535981776011502,4.75540507774079));
#8100=CARTESIAN_POINT('Ctrl Pts',(7.31601994074765,-0.0557826574189054,
4.52663770463754));
#8101=CARTESIAN_POINT('Ctrl Pts',(7.354222969087,0.448762644999277,4.68474223075386));
#8102=CARTESIAN_POINT('Ctrl Pts',(7.39224226780421,0.710217511679504,5.14133781559877));
#8103=CARTESIAN_POINT('Ctrl Pts',(7.43008902366988,0.5916594052894,5.65206211899789));
#8104=CARTESIAN_POINT('Ctrl Pts',(7.4614980372404,0.231764021629228,5.89497907260121));
#8105=CARTESIAN_POINT('Ctrl Pts',(7.48654869737898,-0.0973240615553253,
5.9052786006524));
#8106=CARTESIAN_POINT('Ctrl Pts',(7.50738456391928,-0.355323659444364,5.81476648546977));
#8107=CARTESIAN_POINT('Ctrl Pts',(7.53026554544261,-0.572856338749848,5.60142020877485));
#8108=CARTESIAN_POINT('Ctrl Pts',(7.55517056925149,-0.669836218441959,5.28435098152571));
#8109=CARTESIAN_POINT('Ctrl Pts',(7.57588102694464,-0.614317827947794,5.01429935338668));
#8110=CARTESIAN_POINT('Ctrl Pts',(7.59242404307814,-0.497025790221269,4.83395433811505));
#8111=CARTESIAN_POINT('Ctrl Pts',(7.6089536687432,-0.339149431178674,4.68774659297558));
#8112=CARTESIAN_POINT('Ctrl Pts',(7.62959668968493,-0.0836344771110079,
4.58817926603548));
#8113=CARTESIAN_POINT('Ctrl Pts',(7.65844010764145,0.298170598732022,4.63573436796571));
#8114=CARTESIAN_POINT('Ctrl Pts',(7.68518935302475,0.568322726393191,4.88764401261463));
#8115=CARTESIAN_POINT('Ctrl Pts',(7.70984650366045,0.650261419625715,5.20136259590943));
#8116=CARTESIAN_POINT('Ctrl Pts',(7.7344907134544,0.615036584967239,5.5228070000813));
#8117=CARTESIAN_POINT('Ctrl Pts',(7.76527474802387,0.349308839296457,5.8559972266997));
#8118=CARTESIAN_POINT('Ctrl Pts',(7.79911144782391,-0.113753064206836,5.92449976127185));
#8119=CARTESIAN_POINT('Ctrl Pts',(7.82986619410816,-0.474773880924156,5.72362564992567));
#8120=CARTESIAN_POINT('Ctrl Pts',(7.85755227579443,-0.654292059961964,5.39855675400986));
#8121=CARTESIAN_POINT('Ctrl Pts',(7.87832541447077,-0.638370401196948,5.12017204060674));
#8122=CARTESIAN_POINT('Ctrl Pts',(7.89217334819649,-0.567221155458292,4.95572879884478));
#8123=CARTESIAN_POINT('Ctrl Pts',(7.89909834733727,-0.520617423747659,4.87924437693166));
#8124=CARTESIAN_POINT('Ctrl Pts',(7.90602450006169,-0.46370339051325,4.80995566767418));
#8125=CARTESIAN_POINT('Ctrl Pts',(7.91680097396861,-0.361054204005317,4.71586067278074));
#8126=CARTESIAN_POINT('Ctrl Pts',(7.93759389399371,-0.119518166224153,4.58675402992836));
#8127=CARTESIAN_POINT('Ctrl Pts',(7.96534006210386,0.26236475600673,4.61568621451773));
#8128=CARTESIAN_POINT('Ctrl Pts',(7.99622107554029,0.571693519917959,4.89331989674528));
#8129=CARTESIAN_POINT('Ctrl Pts',(8.02405932467958,0.675115995227338,5.25172945407709));
#8130=CARTESIAN_POINT('Ctrl Pts',(8.05194395308582,0.571652421174932,5.61172186136834));
#8131=CARTESIAN_POINT('Ctrl Pts',(8.07988411081677,0.292101156534909,5.86164971137292));
#8132=CARTESIAN_POINT('Ctrl Pts',(8.10788501784531,-0.0784233387711395,
5.92490818089582));
#8133=CARTESIAN_POINT('Ctrl Pts',(8.13595344261398,-0.426656560206351,5.78097145446324));
#8134=CARTESIAN_POINT('Ctrl Pts',(8.16409525054265,-0.645567978861292,5.47308673944232));
#8135=CARTESIAN_POINT('Ctrl Pts',(8.19231648013073,-0.667238707993714,5.09484527058636));
#8136=CARTESIAN_POINT('Ctrl Pts',(8.22062287004232,-0.483851359843703,4.76202254371853));
#8137=CARTESIAN_POINT('Ctrl Pts',(8.24902004521049,-0.150460572151325,4.57713441531565));
#8138=CARTESIAN_POINT('Ctrl Pts',(8.27751345201596,0.231494106069571,4.59797138762446));
#8139=CARTESIAN_POINT('Ctrl Pts',(8.30610832696761,0.544962336065687,4.81956979365873));
#8140=CARTESIAN_POINT('Ctrl Pts',(8.33480976434835,0.69310132607455,5.17527118660301));
#8141=CARTESIAN_POINT('Ctrl Pts',(8.36362257168318,0.629073409022718,5.55677031488762));
#8142=CARTESIAN_POINT('Ctrl Pts',(8.3925515424265,0.370948750229092,5.84689628452807));
#8143=CARTESIAN_POINT('Ctrl Pts',(8.42160081890503,-0.00363259840954581,
5.95581045784778));
#8144=CARTESIAN_POINT('Ctrl Pts',(8.44591291482813,-0.317350461105933,5.86608437702079));
#8145=CARTESIAN_POINT('Ctrl Pts',(8.46542612591725,-0.511837377716034,5.70209791662713));
#8146=CARTESIAN_POINT('Ctrl Pts',(8.48389640313918,-0.646235426932618,5.50240070801776));
#8147=CARTESIAN_POINT('Ctrl Pts',(8.50623968962513,-0.706096395161048,5.21093606001156));
#8148=CARTESIAN_POINT('Ctrl Pts',(8.5325044635867,-0.603771630310612,4.87662564951356));
#8149=CARTESIAN_POINT('Ctrl Pts',(8.55668059344481,-0.374029117623404,4.65097664338371));
#8150=CARTESIAN_POINT('Ctrl Pts',(8.5787403647823,-0.100834246650297,4.555251023442));
#8151=CARTESIAN_POINT('Ctrl Pts',(8.60529688102436,0.248141502636759,4.56592896275675));
#8152=CARTESIAN_POINT('Ctrl Pts',(8.63865284797812,0.63073545090754,4.82357537459606));
#8153=CARTESIAN_POINT('Ctrl Pts',(8.67894294821516,0.757069626679118,5.36759646206742));
#8154=CARTESIAN_POINT('Ctrl Pts',(8.71950063159077,0.478476625654173,5.85482636408642));
#8155=CARTESIAN_POINT('Ctrl Pts',(8.76033010054568,-0.0612231371037712,
6.0242021516719));
#8156=CARTESIAN_POINT('Ctrl Pts',(8.79458253319758,-0.488965462755427,5.81992360842052));
#8157=CARTESIAN_POINT('Ctrl Pts',(8.82212390948946,-0.681160794137239,5.5136406662995));
#8158=CARTESIAN_POINT('Ctrl Pts',(8.84975893027925,-0.751796896761062,5.1571792721246));
#8159=CARTESIAN_POINT('Ctrl Pts',(8.87984444837189,-0.602041078690657,4.76948039106712));
#8160=CARTESIAN_POINT('Ctrl Pts',(8.91242785081629,-0.237384194390308,4.53301014325183));
#8161=CARTESIAN_POINT('Ctrl Pts',(8.94047881699228,0.134466585038931,4.50317155345517));
#8162=CARTESIAN_POINT('Ctrl Pts',(8.96982711252411,0.491781010059867,4.66232849803431));
#8163=CARTESIAN_POINT('Ctrl Pts',(9.00048403532161,0.731620029022094,4.99675916496741));
#8164=CARTESIAN_POINT('Ctrl Pts',(9.03247511104355,0.75794664861164,5.42565043938059));
#8165=CARTESIAN_POINT('Ctrl Pts',(9.06461825742226,0.551078368819278,5.80448348845649));
#8166=CARTESIAN_POINT('Ctrl Pts',(9.09690994076132,0.172623636920341,6.01627057338027));
#8167=CARTESIAN_POINT('Ctrl Pts',(9.12935177960436,-0.262514946567701,5.99415428011165));
#8168=CARTESIAN_POINT('Ctrl Pts',(9.16193014094924,-0.620844213656014,5.74284535005782));
#8169=CARTESIAN_POINT('Ctrl Pts',(9.19466437324471,-0.791343274428717,5.33760912799968));
#8170=CARTESIAN_POINT('Ctrl Pts',(9.22749713604095,-0.719879593774102,4.90194850755568));
#8171=CARTESIAN_POINT('Ctrl Pts',(9.26053924327341,-0.426350462849809,4.56952461792616));
#8172=CARTESIAN_POINT('Ctrl Pts',(9.2880208954263,-0.0705095289102926,4.46489634881681));
#8173=CARTESIAN_POINT('Ctrl Pts',(9.31031394458354,0.215835839245267,4.50415210664416));
#8174=CARTESIAN_POINT('Ctrl Pts',(9.33210485242398,0.481055339319739,4.62046584167929));
#8175=CARTESIAN_POINT('Ctrl Pts',(9.35556651022956,0.681566722795924,4.84232209585076));
#8176=CARTESIAN_POINT('Ctrl Pts',(9.37372634427259,0.76013142053573,5.0847068874864));
#8177=CARTESIAN_POINT('Ctrl Pts',(9.38691189586978,0.775186012058393,5.22951776549698));
#8178=CARTESIAN_POINT('Ctrl Pts',(9.39044111391715,0.771934376682021,5.31522516777114));
#8179=CARTESIAN_POINT('Ctrl Pts',(9.39232430774748,0.761663575933829,5.38868371146561));
#8180=CARTESIAN_POINT('Ctrl Pts',(9.39470301848468,0.750125538816929,5.44185526499922));
#8181=CARTESIAN_POINT('Ctrl Pts',(9.39675915672847,0.735128865991617,5.4937547021154));
#8182=CARTESIAN_POINT('Ctrl Pts',(9.40062547913648,0.697631703938273,5.59576957012101));
#8183=CARTESIAN_POINT('Ctrl Pts',(9.40678906395115,0.614761668799333,5.73804352075162));
#8184=CARTESIAN_POINT('Ctrl Pts',(9.41479721859882,0.455844412061066,5.88979323730855));
#8185=CARTESIAN_POINT('Ctrl Pts',(9.42290476320863,0.260938548878604,5.99172438224085));
#8186=CARTESIAN_POINT('Ctrl Pts',(9.43098028733991,0.0452935297457695,6.03554040196323));
#8187=CARTESIAN_POINT('Ctrl Pts',(9.44178112627354,-0.24759975779143,6.01245735507339));
#8188=CARTESIAN_POINT('Ctrl Pts',(9.45527918626336,-0.579717863548197,5.83096339648743));
#8189=CARTESIAN_POINT('Ctrl Pts',(9.47151748582056,-0.801334910259173,5.43325751280776));
#8190=CARTESIAN_POINT('Ctrl Pts',(9.48777877066663,-0.777156535330782,4.97819185288487));
#8191=CARTESIAN_POINT('Ctrl Pts',(9.50406651147499,-0.514028895195191,4.60503104228514));
#8192=CARTESIAN_POINT('Ctrl Pts',(9.52038183374562,-0.0919082290386587,
4.42949936533505));
#8193=CARTESIAN_POINT('Ctrl Pts',(9.53672456739186,0.35951284935727,4.5052776841562));
#8194=CARTESIAN_POINT('Ctrl Pts',(9.55308672779057,0.70168150119454,4.81072784092244));
#8195=CARTESIAN_POINT('Ctrl Pts',(9.56401498954576,0.786439952711774,5.10433647990876));
#8196=CARTESIAN_POINT('Ctrl Pts',(9.56947716492856,0.786459812675507,5.25186167987965));
#8197=CARTESIAN_POINT('Ctrl Pts',(6.53728986429481,0.791457584369433,5.24788844117082));
#8198=CARTESIAN_POINT('Ctrl Pts',(6.54278417054037,0.791437607580227,5.39628144910989));
#8199=CARTESIAN_POINT('Ctrl Pts',(6.55378249785739,0.706095273707095,5.69170633675433));
#8200=CARTESIAN_POINT('Ctrl Pts',(6.57024265516649,0.36194294842202,5.99886043512873));
#8201=CARTESIAN_POINT('Ctrl Pts',(6.58668071586564,-0.0921185468821841,
6.07520217151));
#8202=CARTESIAN_POINT('Ctrl Pts',(6.60308941390448,-0.516358086898658,5.8984073300043));
#8203=CARTESIAN_POINT('Ctrl Pts',(6.61947110658782,-0.781148791011006,5.52353693808151));
#8204=CARTESIAN_POINT('Ctrl Pts',(6.63582102071739,-0.805316342370628,5.06602826377862));
#8205=CARTESIAN_POINT('Ctrl Pts',(6.65214502140613,-0.582650139481846,4.66642310779825));
#8206=CARTESIAN_POINT('Ctrl Pts',(6.66571399431892,-0.248901893197726,4.48404923727362));
#8207=CARTESIAN_POINT('Ctrl Pts',(6.67656588894199,0.0453190981676558,4.46087101406537));
#8208=CARTESIAN_POINT('Ctrl Pts',(6.68467931966452,0.261934715600987,4.50488378698986));
#8209=CARTESIAN_POINT('Ctrl Pts',(6.69282445640136,0.457697749274946,4.60726786189105));
#8210=CARTESIAN_POINT('Ctrl Pts',(6.70086847028765,0.617302246342184,4.75966820326596));
#8211=CARTESIAN_POINT('Ctrl Pts',(6.70706046107289,0.700528406866124,4.90254788180947));
#8212=CARTESIAN_POINT('Ctrl Pts',(6.71094234002084,0.73818000698364,5.00497270204404));
#8213=CARTESIAN_POINT('Ctrl Pts',(6.71300604048302,0.753222836061835,5.05704788335984));
#8214=CARTESIAN_POINT('Ctrl Pts',(6.71539366913855,0.764820751174518,5.11043973498399));
#8215=CARTESIAN_POINT('Ctrl Pts',(6.71729493969799,0.77513823533657,5.18438795256581));
#8216=CARTESIAN_POINT('Ctrl Pts',(6.72080892065097,0.778397838898288,5.26987667291114));
#8217=CARTESIAN_POINT('Ctrl Pts',(6.73404917601244,0.763282472885072,5.4153514076569));
#8218=CARTESIAN_POINT('Ctrl Pts',(6.75227750605218,0.684423920730263,5.65860295458565));
#8219=CARTESIAN_POINT('Ctrl Pts',(6.77583192680458,0.483163536120546,5.8812916764581));
#8220=CARTESIAN_POINT('Ctrl Pts',(6.79769115526016,0.217124051184817,5.99794934103775));
#8221=CARTESIAN_POINT('Ctrl Pts',(6.8200508970381,-0.0700279426602678,6.03731900340549));
#8222=CARTESIAN_POINT('Ctrl Pts',(6.84761039460488,-0.426870037969381,5.93241072619413));
#8223=CARTESIAN_POINT('Ctrl Pts',(6.87950319278275,-0.70993595670243,5.61157204292273));
#8224=CARTESIAN_POINT('Ctrl Pts',(6.90997077663386,-0.788035834470172,5.21287382442806));
#8225=CARTESIAN_POINT('Ctrl Pts',(6.93913173491947,-0.671557590403463,4.84250449492373));
#8226=CARTESIAN_POINT('Ctrl Pts',(6.96815537921053,-0.393284210691007,4.57391816840494));
#8227=CARTESIAN_POINT('Ctrl Pts',(6.99706486303965,-0.0221876157039304,
4.47165816386748));
#8228=CARTESIAN_POINT('Ctrl Pts',(7.02584295552157,0.350991457602562,4.55877532096753));
#8229=CARTESIAN_POINT('Ctrl Pts',(7.05210448870892,0.612009659039021,4.79186963182615));
#8230=CARTESIAN_POINT('Ctrl Pts',(7.07588277971234,0.734898688262069,5.07852803586258));
#8231=CARTESIAN_POINT('Ctrl Pts',(7.10431766120651,0.748473408452173,5.45246510432511));
#8232=CARTESIAN_POINT('Ctrl Pts',(7.13495982630399,0.534772722166524,5.81756547683734));
#8233=CARTESIAN_POINT('Ctrl Pts',(7.16776257929051,0.13488149437605,5.99479462816283));
#8234=CARTESIAN_POINT('Ctrl Pts',(7.19574440030138,-0.236141062682786,5.96531940176238));
#8235=CARTESIAN_POINT('Ctrl Pts',(7.2177901342577,-0.482095505862949,5.8048713584837));
#8236=CARTESIAN_POINT('Ctrl Pts',(7.23397954190281,-0.609110618529052,5.63776724940332));
#8237=CARTESIAN_POINT('Ctrl Pts',(7.24783086290047,-0.689316230456583,5.47725973143276));
#8238=CARTESIAN_POINT('Ctrl Pts',(7.27200410720517,-0.748321146352422,5.16483188372505));
#8239=CARTESIAN_POINT('Ctrl Pts',(7.30634760775194,-0.573092566975053,4.72345680527967));
#8240=CARTESIAN_POINT('Ctrl Pts',(7.34725724358845,-0.061282166766824,4.47987864397431));
#8241=CARTESIAN_POINT('Ctrl Pts',(7.38786714614943,0.475093187126763,4.64821747196133));
#8242=CARTESIAN_POINT('Ctrl Pts',(7.4281808884662,0.752162744425484,5.13262048509692));
#8243=CARTESIAN_POINT('Ctrl Pts',(7.4682032841975,0.626465961329015,5.67275193455503));
#8244=CARTESIAN_POINT('Ctrl Pts',(7.50131695661259,0.246792245186754,5.92871444590393));
#8245=CARTESIAN_POINT('Ctrl Pts',(7.5276686028738,-0.0994340094365663,5.93948771421208));
#8246=CARTESIAN_POINT('Ctrl Pts',(7.54955183986769,-0.370434232319783,5.84438053773469));
#8247=CARTESIAN_POINT('Ctrl Pts',(7.57352589450599,-0.598389487794979,5.62068677638571));
#8248=CARTESIAN_POINT('Ctrl Pts',(7.59956122744709,-0.699716036243272,5.28908655646374));
#8249=CARTESIAN_POINT('Ctrl Pts',(7.62116131797656,-0.641707280988357,5.00738066570936));
#8250=CARTESIAN_POINT('Ctrl Pts',(7.63838529282816,-0.51956007976562,4.81959623297834));
#8251=CARTESIAN_POINT('Ctrl Pts',(7.65557203307511,-0.355360709732147,4.66755759217184));
#8252=CARTESIAN_POINT('Ctrl Pts',(7.67698583504015,-0.0901629384316624,
4.56431184492957));
#8253=CARTESIAN_POINT('Ctrl Pts',(7.7068428996256,0.305080740614273,4.61367696897994));
#8254=CARTESIAN_POINT('Ctrl Pts',(7.73442574632612,0.583537909728163,4.87373760666019));
#8255=CARTESIAN_POINT('Ctrl Pts',(7.75977754006825,0.667718615594098,5.19632076194103));
#8256=CARTESIAN_POINT('Ctrl Pts',(7.78505717843533,0.631510008529416,5.52614830373602));
#8257=CARTESIAN_POINT('Ctrl Pts',(7.81652540185333,0.359488412685916,5.86663423903951));
#8258=CARTESIAN_POINT('Ctrl Pts',(7.8509623942454,-0.11195737754036,5.93596459383563));
#8259=CARTESIAN_POINT('Ctrl Pts',(7.88213634505837,-0.477884403820245,5.73212312446919));
#8260=CARTESIAN_POINT('Ctrl Pts',(7.91009554163285,-0.659080145871757,5.40362312816743));
#8261=CARTESIAN_POINT('Ctrl Pts',(7.93099687270145,-0.642907181436071,5.12339682980178));
#8262=CARTESIAN_POINT('Ctrl Pts',(7.94490706513547,-0.571422723993177,4.95820274283118));
#8263=CARTESIAN_POINT('Ctrl Pts',(7.95185706711927,-0.524643983980393,4.8814350077215));
#8264=CARTESIAN_POINT('Ctrl Pts',(7.95880208822775,-0.467565899481637,4.81195386368381));
#8265=CARTESIAN_POINT('Ctrl Pts',(7.96959766060679,-0.364723690059826,4.71768110428399));
#8266=CARTESIAN_POINT('Ctrl Pts',(7.99039050550677,-0.123078463851595,4.58860653829953));
#8267=CARTESIAN_POINT('Ctrl Pts',(8.01804399168185,0.257517145674564,4.61775924801183));
#8268=CARTESIAN_POINT('Ctrl Pts',(8.04868561583974,0.564353076015046,4.89347251399917));
#8269=CARTESIAN_POINT('Ctrl Pts',(8.07620529241276,0.666448377061362,5.24794644083153));
#8270=CARTESIAN_POINT('Ctrl Pts',(8.10367692972224,0.564301163146253,5.60265220795495));
#8271=CARTESIAN_POINT('Ctrl Pts',(8.1311063371322,0.289652716430529,5.84793638333599));
#8272=CARTESIAN_POINT('Ctrl Pts',(8.15850125893085,-0.0729805081161587,
5.90966061766628));
#8273=CARTESIAN_POINT('Ctrl Pts',(8.18586870658201,-0.412536152354017,5.76911441682784));
#8274=CARTESIAN_POINT('Ctrl Pts',(8.2132161293016,-0.625176848653941,5.46974735708836));
#8275=CARTESIAN_POINT('Ctrl Pts',(8.24055084302331,-0.64600120604342,5.10329359763361));
#8276=CARTESIAN_POINT('Ctrl Pts',(8.26788027572269,-0.468758984456337,4.78196882475003));
#8277=CARTESIAN_POINT('Ctrl Pts',(8.29521182844757,-0.147733887802402,4.60412415342451));
#8278=CARTESIAN_POINT('Ctrl Pts',(8.32255291725131,0.218837928434283,4.62428040570159));
#8279=CARTESIAN_POINT('Ctrl Pts',(8.34991094871533,0.51871581464964,4.83645895467768));
#8280=CARTESIAN_POINT('Ctrl Pts',(8.37729320920923,0.659936333003741,5.17593146088852));
#8281=CARTESIAN_POINT('Ctrl Pts',(8.40470716926229,0.598866621643475,5.53894810421618));
#8282=CARTESIAN_POINT('Ctrl Pts',(8.43215968688036,0.353772456268368,5.81422753527536));
#8283=CARTESIAN_POINT('Ctrl Pts',(8.45965873301394,-0.00090935564745819,
5.91721890831774));
#8284=CARTESIAN_POINT('Ctrl Pts',(8.48261763222319,-0.297193347524019,5.832373515472));
#8285=CARTESIAN_POINT('Ctrl Pts',(8.5010170841175,-0.480578633759046,5.67772295629852));
#8286=CARTESIAN_POINT('Ctrl Pts',(8.51841470498558,-0.607165316349347,5.48959928016275));
#8287=CARTESIAN_POINT('Ctrl Pts',(8.53942561001488,-0.663406845956722,5.21544933331551));
#8288=CARTESIAN_POINT('Ctrl Pts',(8.5640860352834,-0.567257575299942,4.9015656424331));
#8289=CARTESIAN_POINT('Ctrl Pts',(8.5867469390981,-0.351851325775005,4.69008336352928));
#8290=CARTESIAN_POINT('Ctrl Pts',(8.60739743163042,-0.096086131236525,4.60049517355307));
#8291=CARTESIAN_POINT('Ctrl Pts',(8.63223189061381,0.230279583670253,4.6105197427705));
#8292=CARTESIAN_POINT('Ctrl Pts',(8.66337612152979,0.587448284147565,4.85122937163191));
#8293=CARTESIAN_POINT('Ctrl Pts',(8.70092976062667,0.705041399270903,5.35836385208443));
#8294=CARTESIAN_POINT('Ctrl Pts',(8.73867762820808,0.445619450565281,5.81178687736278));
#8295=CARTESIAN_POINT('Ctrl Pts',(8.77663330730281,-0.0561408892919382,
5.96913573334488));
#8296=CARTESIAN_POINT('Ctrl Pts',(8.808445476751,-0.453384395196325,5.77934323807869));
#8297=CARTESIAN_POINT('Ctrl Pts',(8.83401240846527,-0.631791197131727,5.49501245739173));
#8298=CARTESIAN_POINT('Ctrl Pts',(8.85965950209186,-0.697335209574664,5.16418731265143));
#8299=CARTESIAN_POINT('Ctrl Pts',(8.88757321050643,-0.558369116925368,4.80448896156448));
#8300=CARTESIAN_POINT('Ctrl Pts',(8.91780053797859,-0.220082182336464,4.58512097737996));
#8301=CARTESIAN_POINT('Ctrl Pts',(8.94382442090338,0.124888837012952,4.5574388084705));
#8302=CARTESIAN_POINT('Ctrl Pts',(8.97105550892288,0.456421745283963,4.7051036988583));
#8303=CARTESIAN_POINT('Ctrl Pts',(8.99951073066361,0.67902904616484,5.01548343676037));
#8304=CARTESIAN_POINT('Ctrl Pts',(9.02921638462349,0.703497102878303,5.41370372897262));
#8305=CARTESIAN_POINT('Ctrl Pts',(9.05908029308652,0.511342876044629,5.76565926471648));
#8306=CARTESIAN_POINT('Ctrl Pts',(9.08910308021335,0.159530985782651,5.96258159182352));
#8307=CARTESIAN_POINT('Ctrl Pts',(9.1192905439651,-0.245331677769252,5.94205029820737));
#8308=CARTESIAN_POINT('Ctrl Pts',(9.14963403851829,-0.579074368916519,5.70804769353886));
#8309=CARTESIAN_POINT('Ctrl Pts',(9.18015561858369,-0.738086143309763,5.33026750887227));
#8310=CARTESIAN_POINT('Ctrl Pts',(9.21080588468753,-0.671444952751785,4.92359816795805));
#8311=CARTESIAN_POINT('Ctrl Pts',(9.24169181514135,-0.39715715916767,4.61285379721767));
#8312=CARTESIAN_POINT('Ctrl Pts',(9.26741765382922,-0.0641141613479425,
4.51484111966771));
#8313=CARTESIAN_POINT('Ctrl Pts',(9.2883080329795,0.20420407129801,4.55162436548779));
#8314=CARTESIAN_POINT('Ctrl Pts',(9.30874254903957,0.452902156553228,4.66063468512768));
#8315=CARTESIAN_POINT('Ctrl Pts',(9.33077742980449,0.641269387174206,4.86904883099884));
#8316=CARTESIAN_POINT('Ctrl Pts',(9.34785549284168,0.715152744632072,5.0968004916225));
#8317=CARTESIAN_POINT('Ctrl Pts',(9.3602755301295,0.729323789248401,5.23347950840958));
#8318=CARTESIAN_POINT('Ctrl Pts',(9.36347417466056,0.726285408376634,5.31181320851451));
#8319=CARTESIAN_POINT('Ctrl Pts',(9.3652893660282,0.716598586410511,5.38174950648743));
#8320=CARTESIAN_POINT('Ctrl Pts',(9.36752488741168,0.705685048065471,5.43181944939317));
#8321=CARTESIAN_POINT('Ctrl Pts',(9.3694564647943,0.691630806425038,5.48052738798772));
#8322=CARTESIAN_POINT('Ctrl Pts',(9.37309440175116,0.656329841837037,5.57653790841529));
#8323=CARTESIAN_POINT('Ctrl Pts',(9.37890017016595,0.578305869960337,5.71051132408279));
#8324=CARTESIAN_POINT('Ctrl Pts',(9.38644471609761,0.428595584489612,5.85346785080748));
#8325=CARTESIAN_POINT('Ctrl Pts',(9.39408703335625,0.244909855550526,5.94954069523186));
#8326=CARTESIAN_POINT('Ctrl Pts',(9.40170234262852,0.0415804244967724,5.99086118264962));
#8327=CARTESIAN_POINT('Ctrl Pts',(9.41189201019065,-0.234704618905985,5.96909752603866));
#8328=CARTESIAN_POINT('Ctrl Pts',(9.42463859874445,-0.548259442305881,5.79780663399558));
#8329=CARTESIAN_POINT('Ctrl Pts',(9.43998582035194,-0.757710474392766,5.42204388560271));
#8330=CARTESIAN_POINT('Ctrl Pts',(9.4553698847925,-0.734901408935396,4.99163053542099));
#8331=CARTESIAN_POINT('Ctrl Pts',(9.47079546212505,-0.485807828284844,4.638295123357));
#8332=CARTESIAN_POINT('Ctrl Pts',(9.48626038209685,-0.0857752245725713,
4.47188596344179));
#8333=CARTESIAN_POINT('Ctrl Pts',(9.50176629783407,0.342505541926648,4.54371374658917));
#8334=CARTESIAN_POINT('Ctrl Pts',(9.51730779271675,0.667520614060755,4.83376258154226));
#8335=CARTESIAN_POINT('Ctrl Pts',(9.52769881073733,0.748180309761582,5.11286768976882));
#8336=CARTESIAN_POINT('Ctrl Pts',(9.53289545467617,0.748199204277581,5.25322128197838));
#8337=CARTESIAN_POINT('Ctrl Pts',(6.45999557459768,0.809254259106663,5.250752686764));
#8338=CARTESIAN_POINT('Ctrl Pts',(6.4656153380923,0.809233826166506,5.40253410767546));
#8339=CARTESIAN_POINT('Ctrl Pts',(6.47687026388547,0.721996890342757,5.70493974187684));
#8340=CARTESIAN_POINT('Ctrl Pts',(6.49375251888294,0.369096209330993,6.02010570850611));
#8341=CARTESIAN_POINT('Ctrl Pts',(6.51064436532253,-0.0975430423797339,
6.09868870265511));
#8342=CARTESIAN_POINT('Ctrl Pts',(6.52754122332568,-0.534494623907844,5.91673254754402));
#8343=CARTESIAN_POINT('Ctrl Pts',(6.54444265909054,-0.80783698079355,5.52997825893372));
#8344=CARTESIAN_POINT('Ctrl Pts',(6.56134181204163,-0.832953247332849,5.05695964598303));
#8345=CARTESIAN_POINT('Ctrl Pts',(6.57824957990225,-0.602395099269935,4.64291194589478));
#8346=CARTESIAN_POINT('Ctrl Pts',(6.59232904971087,-0.256033804084603,4.45351553617427));
#8347=CARTESIAN_POINT('Ctrl Pts',(6.60360883315493,0.0498248485384295,4.42939603265042));
#8348=CARTESIAN_POINT('Ctrl Pts',(6.61205006886682,0.275217590098315,4.47517626334091));
#8349=CARTESIAN_POINT('Ctrl Pts',(6.62053196867004,0.479123848697043,4.58179723556108));
#8350=CARTESIAN_POINT('Ctrl Pts',(6.62891789718303,0.645505596832454,4.74066879125782));
#8351=CARTESIAN_POINT('Ctrl Pts',(6.63537635713297,0.732382034014202,4.88975766855534));
#8352=CARTESIAN_POINT('Ctrl Pts',(6.63943352928247,0.771687074389179,4.99674959091469));
#8353=CARTESIAN_POINT('Ctrl Pts',(6.64159806006668,0.787546974765718,5.05148060438962));
#8354=CARTESIAN_POINT('Ctrl Pts',(6.64410012271561,0.799529214601232,5.10718632608853));
#8355=CARTESIAN_POINT('Ctrl Pts',(6.64598144448542,0.810256089987908,5.18246997920793));
#8356=CARTESIAN_POINT('Ctrl Pts',(6.64995259301237,0.813716246088648,5.27746723531887));
#8357=CARTESIAN_POINT('Ctrl Pts',(6.66376398254105,0.797925459082292,5.42854929342793));
#8358=CARTESIAN_POINT('Ctrl Pts',(6.68284421486437,0.715379131781609,5.68363809114948));
#8359=CARTESIAN_POINT('Ctrl Pts',(6.70758451472148,0.504157330037584,5.9173892723336));
#8360=CARTESIAN_POINT('Ctrl Pts',(6.73061771554503,0.223813352606992,6.04046536159552));
#8361=CARTESIAN_POINT('Ctrl Pts',(6.75422019989529,-0.0793026005240917,
6.08203779050005));
#8362=CARTESIAN_POINT('Ctrl Pts',(6.783391300017,-0.457122076023753,5.97122820611254));
#8363=CARTESIAN_POINT('Ctrl Pts',(6.81727322163079,-0.758063258382887,5.63048355896042));
#8364=CARTESIAN_POINT('Ctrl Pts',(6.84975212437726,-0.84150197430614,5.20546023039942));
#8365=CARTESIAN_POINT('Ctrl Pts',(6.88093505637388,-0.717082698284182,4.80931695387591));
#8366=CARTESIAN_POINT('Ctrl Pts',(6.91206488791777,-0.418682655365162,4.52109212196899));
#8367=CARTESIAN_POINT('Ctrl Pts',(6.94316889035763,-0.0194331785847506,
4.41091747648985));
#8368=CARTESIAN_POINT('Ctrl Pts',(6.97422006674403,0.383283395774545,4.5047807265211));
#8369=CARTESIAN_POINT('Ctrl Pts',(7.00263321675371,0.665816074281837,4.75690914542035));
#8370=CARTESIAN_POINT('Ctrl Pts',(7.02842338889131,0.799161055122401,5.06782415611563));
#8371=CARTESIAN_POINT('Ctrl Pts',(7.05932459014209,0.814003215770462,5.47420123361874));
#8372=CARTESIAN_POINT('Ctrl Pts',(7.09271704357918,0.581339250156787,5.87227691308354));
#8373=CARTESIAN_POINT('Ctrl Pts',(7.12857742875714,0.144206008983758,6.0661807345317));
#8374=CARTESIAN_POINT('Ctrl Pts',(7.15923642529593,-0.262355703606541,6.03398209938642));
#8375=CARTESIAN_POINT('Ctrl Pts',(7.18344185505573,-0.532486116512524,5.85786320372732));
#8376=CARTESIAN_POINT('Ctrl Pts',(7.2012453498512,-0.672177603901523,5.67409256107297));
#8377=CARTESIAN_POINT('Ctrl Pts',(7.21648898591514,-0.760453017446425,5.49744398399632));
#8378=CARTESIAN_POINT('Ctrl Pts',(7.24312182063594,-0.825515825922649,5.15323254742201));
#8379=CARTESIAN_POINT('Ctrl Pts',(7.28103894373652,-0.632275153963754,4.665803037915));
#8380=CARTESIAN_POINT('Ctrl Pts',(7.3263220317354,-0.0658377557766746,4.39591133185141));
#8381=CARTESIAN_POINT('Ctrl Pts',(7.37137511216033,0.52933208569028,4.58245170719848));
#8382=CARTESIAN_POINT('Ctrl Pts',(7.41618714911392,0.837507063114166,5.12082756912408));
#8383=CARTESIAN_POINT('Ctrl Pts',(7.46074788044844,0.697712679683577,5.7222691996181));
#8384=CARTESIAN_POINT('Ctrl Pts',(7.49766411510097,0.274482978524602,6.00771346693692));
#8385=CARTESIAN_POINT('Ctrl Pts',(7.52706281789054,-0.111787067247916,6.01974462374398));
#8386=CARTESIAN_POINT('Ctrl Pts',(7.55148599389226,-0.414241243525464,5.9136075100233));
#8387=CARTESIAN_POINT('Ctrl Pts',(7.57825173171333,-0.668747225075187,5.66387265100419));
#8388=CARTESIAN_POINT('Ctrl Pts',(7.60732576554949,-0.781899451692313,5.29357550966227));
#8389=CARTESIAN_POINT('Ctrl Pts',(7.63144825543078,-0.717112820017105,4.97897772631035));
#8390=CARTESIAN_POINT('Ctrl Pts',(7.65068202749864,-0.580711872249469,4.76928606869434));
#8391=CARTESIAN_POINT('Ctrl Pts',(7.66987254015019,-0.397368841933043,4.59952785513379));
#8392=CARTESIAN_POINT('Ctrl Pts',(7.6937789668775,-0.101308809637811,4.48428345691279));
#8393=CARTESIAN_POINT('Ctrl Pts',(7.72709483698664,0.339719003758443,4.53940207795531));
#8394=CARTESIAN_POINT('Ctrl Pts',(7.75785104299278,0.650135480752808,4.82942921168495));
#8395=CARTESIAN_POINT('Ctrl Pts',(7.78609058120298,0.743868677952219,5.18874820762418));
#8396=CARTESIAN_POINT('Ctrl Pts',(7.81422927914199,0.703540142915436,5.5558670520897));
#8397=CARTESIAN_POINT('Ctrl Pts',(7.84921332159718,0.401011003875481,5.93425427218728));
#8398=CARTESIAN_POINT('Ctrl Pts',(7.88741640054593,-0.121987511272621,6.01093434276299));
#8399=CARTESIAN_POINT('Ctrl Pts',(7.92192473853693,-0.526942532140401,5.78518530972292));
#8400=CARTESIAN_POINT('Ctrl Pts',(7.95281213238897,-0.726978532166836,5.42226623438594));
#8401=CARTESIAN_POINT('Ctrl Pts',(7.97585068557117,-0.709046349578469,5.11344268985378));
#8402=CARTESIAN_POINT('Ctrl Pts',(7.99115589437824,-0.630392934079408,4.93169356901783));
#8403=CARTESIAN_POINT('Ctrl Pts',(7.99879796520076,-0.57895613111009,4.84728516828961));
#8404=CARTESIAN_POINT('Ctrl Pts',(8.00642950767667,-0.516235309566051,4.77094091026953));
#8405=CARTESIAN_POINT('Ctrl Pts',(8.01828457552326,-0.403306159141596,4.66742318077098));
#8406=CARTESIAN_POINT('Ctrl Pts',(8.04109084512299,-0.138232407133623,4.52591534703238));
#8407=CARTESIAN_POINT('Ctrl Pts',(8.07133153658797,0.277933340832045,4.55808290998239));
#8408=CARTESIAN_POINT('Ctrl Pts',(8.10472163981035,0.612088745400635,4.85866032793836));
#8409=CARTESIAN_POINT('Ctrl Pts',(8.13461238013838,0.722784116446006,5.24364859132425));
#8410=CARTESIAN_POINT('Ctrl Pts',(8.16434352076723,0.612051583526427,5.62741670623071));
#8411=CARTESIAN_POINT('Ctrl Pts',(8.19391894017278,0.315829296131672,5.89168368886382));
#8412=CARTESIAN_POINT('Ctrl Pts',(8.22334148667717,-0.073615600048539,5.95774627858268));
#8413=CARTESIAN_POINT('Ctrl Pts',(8.2526148686265,-0.436664486169176,5.80722357120211));
#8414=CARTESIAN_POINT('Ctrl Pts',(8.2817428109828,-0.662913169596188,5.48828297433822));
#8415=CARTESIAN_POINT('Ctrl Pts',(8.31072941188433,-0.684744084908157,5.09973973531902));
#8416=CARTESIAN_POINT('Ctrl Pts',(8.33957899299675,-0.497454685626346,4.76072710518954));
#8417=CARTESIAN_POINT('Ctrl Pts',(8.36829613554204,-0.160092402883954,4.57412892458932));
#8418=CARTESIAN_POINT('Ctrl Pts',(8.39688569797962,0.223129005271864,4.59546606782747));
#8419=CARTESIAN_POINT('Ctrl Pts',(8.42535271673465,0.53494485713908,4.81642132873474));
#8420=CARTESIAN_POINT('Ctrl Pts',(8.4537025819109,0.68087147706904,5.16792102261738));
#8421=CARTESIAN_POINT('Ctrl Pts',(8.48194066992712,0.617705346936381,5.54172542134465));
#8422=CARTESIAN_POINT('Ctrl Pts',(8.51007311419913,0.366388819790279,5.82356941025869));
#8423=CARTESIAN_POINT('Ctrl Pts',(8.53810505214009,0.00483044772678114,
5.92826112657717));
#8424=CARTESIAN_POINT('Ctrl Pts',(8.56138803027302,-0.295480207153548,5.84201972788554));
#8425=CARTESIAN_POINT('Ctrl Pts',(8.57996830905769,-0.480604419515746,5.68583764688899));
#8426=CARTESIAN_POINT('Ctrl Pts',(8.59748940753691,-0.608047312296436,5.4963666433294));
#8427=CARTESIAN_POINT('Ctrl Pts',(8.61857918989552,-0.664302447321313,5.221247595173));
#8428=CARTESIAN_POINT('Ctrl Pts',(8.64320525787944,-0.56811782681272,4.90788926095751));
#8429=CARTESIAN_POINT('Ctrl Pts',(8.66573081669197,-0.353908674160115,4.69784543743962));
#8430=CARTESIAN_POINT('Ctrl Pts',(8.6861712326096,-0.100775202667368,4.60925906979357));
#8431=CARTESIAN_POINT('Ctrl Pts',(8.71066377776687,0.221098389390166,4.61926760882404));
#8432=CARTESIAN_POINT('Ctrl Pts',(8.74122227864302,0.571184388107263,4.85585622113353));
#8433=CARTESIAN_POINT('Ctrl Pts',(8.7778130831244,0.685078508551102,5.3500353521348));
#8434=CARTESIAN_POINT('Ctrl Pts',(8.81434182728614,0.433536012261789,5.78839143480342));
#8435=CARTESIAN_POINT('Ctrl Pts',(8.85082537278578,-0.0488556501951366,
5.93899861839975));
#8436=CARTESIAN_POINT('Ctrl Pts',(8.88120666328966,-0.427908344867109,5.75733976610283));
#8437=CARTESIAN_POINT('Ctrl Pts',(8.90550515735323,-0.597345302500117,5.48714044975464));
#8438=CARTESIAN_POINT('Ctrl Pts',(8.92980208102577,-0.65933912822784,5.1737060918429));
#8439=CARTESIAN_POINT('Ctrl Pts',(8.95613036104259,-0.527930599875553,4.83463896743551));
#8440=CARTESIAN_POINT('Ctrl Pts',(8.98449755789417,-0.210401683525278,4.62895776604595));
#8441=CARTESIAN_POINT('Ctrl Pts',(9.0088288410772,0.112116097503262,4.60321902465812));
#8442=CARTESIAN_POINT('Ctrl Pts',(9.03419634827837,0.420871346111283,4.74090449262632));
#8443=CARTESIAN_POINT('Ctrl Pts',(9.06061136980048,0.627320838871634,5.02907173541959));
#8444=CARTESIAN_POINT('Ctrl Pts',(9.0880818259389,0.649761518074933,5.39726951746239));
#8445=CARTESIAN_POINT('Ctrl Pts',(9.11560011871394,0.472584972123624,5.72143515200543));
#8446=CARTESIAN_POINT('Ctrl Pts',(9.14317100932603,0.149484864062567,5.90209915790658));
#8447=CARTESIAN_POINT('Ctrl Pts',(9.17080492383359,-0.221056026697281,5.88315245478754));
#8448=CARTESIAN_POINT('Ctrl Pts',(9.19849913151102,-0.525520480330484,5.66949773032316));
#8449=CARTESIAN_POINT('Ctrl Pts',(9.22627859524352,-0.670094333871429,5.32565914727594));
#8450=CARTESIAN_POINT('Ctrl Pts',(9.25410461778296,-0.609472890704072,4.95654943349016));
#8451=CARTESIAN_POINT('Ctrl Pts',(9.28207813619629,-0.360990719160832,4.67522249318265));
#8452=CARTESIAN_POINT('Ctrl Pts',(9.30533083985056,-0.0599919750808904,
4.58674525641782));
#8453=CARTESIAN_POINT('Ctrl Pts',(9.32418289262162,0.18212513724471,4.619946808137));
#8454=CARTESIAN_POINT('Ctrl Pts',(9.34260730899467,0.406349206044995,4.71826942359272));
#8455=CARTESIAN_POINT('Ctrl Pts',(9.36245403617579,0.575921431786298,4.90591614259015));
#8456=CARTESIAN_POINT('Ctrl Pts',(9.377810035467,0.642356264883323,5.11081796432513));
#8457=CARTESIAN_POINT('Ctrl Pts',(9.38896656846135,0.655091434360625,5.23342471494882));
#8458=CARTESIAN_POINT('Ctrl Pts',(9.39191714275027,0.652347070971567,5.3052545908254));
#8459=CARTESIAN_POINT('Ctrl Pts',(9.3935201178333,0.643661393979997,5.36754984112474));
#8460=CARTESIAN_POINT('Ctrl Pts',(9.39552997481224,0.63389436064975,5.41250038978432));
#8461=CARTESIAN_POINT('Ctrl Pts',(9.39726703478231,0.621234849848933,5.45632929190797));
#8462=CARTESIAN_POINT('Ctrl Pts',(9.40053483057608,0.589538443172086,5.54255337995261));
#8463=CARTESIAN_POINT('Ctrl Pts',(9.40574774560895,0.51947566576292,5.66283951997694));
#8464=CARTESIAN_POINT('Ctrl Pts',(9.41252022585287,0.385101609192844,5.79115143286413));
#8465=CARTESIAN_POINT('Ctrl Pts',(9.41937850660532,0.220268888907917,5.87736017606902));
#8466=CARTESIAN_POINT('Ctrl Pts',(9.42621082062533,0.0378591974212147,5.91442689341244));
#8467=CARTESIAN_POINT('Ctrl Pts',(9.43535036503967,-0.209940808359547,5.89490298832899));
#8468=CARTESIAN_POINT('Ctrl Pts',(9.44678065086537,-0.491072382960274,5.74130501383786));
#8469=CARTESIAN_POINT('Ctrl Pts',(9.46053662841775,-0.678774393287174,5.40451551930697));
#8470=CARTESIAN_POINT('Ctrl Pts',(9.47432096030564,-0.658324053358711,5.01889497646438));
#8471=CARTESIAN_POINT('Ctrl Pts',(9.48813807913884,-0.435204188314633,4.70241739537075));
#8472=CARTESIAN_POINT('Ctrl Pts',(9.50198713723629,-0.0769945315313026,
4.55342872186793));
#8473=CARTESIAN_POINT('Ctrl Pts',(9.51586821916381,0.30642949046769,4.61770812146408));
#8474=CARTESIAN_POINT('Ctrl Pts',(9.52978247204756,0.597360200833237,4.87739913147432));
#8475=CARTESIAN_POINT('Ctrl Pts',(9.53907878780185,0.669558525647519,5.127085468639));
#8476=CARTESIAN_POINT('Ctrl Pts',(9.54373454600902,0.669575453553099,5.25283054498549));
#8477=CARTESIAN_POINT('Ctrl Pts',(6.3975642485275,0.760068228697932,5.2530576083404));
#8478=CARTESIAN_POINT('Ctrl Pts',(6.40284604135377,0.760049024587858,5.39571094613652));
#8479=CARTESIAN_POINT('Ctrl Pts',(6.41342366827503,0.678086500584757,5.67989070809738));
#8480=CARTESIAN_POINT('Ctrl Pts',(6.42932406057163,0.345838155681425,5.97679828638407));
#8481=CARTESIAN_POINT('Ctrl Pts',(6.44525966089941,-0.0943537342223277,
6.05101384381127));
#8482=CARTESIAN_POINT('Ctrl Pts',(6.46122925955391,-0.507332803137623,5.87917628308332));
#8483=CARTESIAN_POINT('Ctrl Pts',(6.47723247686921,-0.766215951571805,5.5130774349882));
#8484=CARTESIAN_POINT('Ctrl Pts',(6.4932655429891,-0.790163937030003,5.06441564556022));
#8485=CARTESIAN_POINT('Ctrl Pts',(6.50933478250395,-0.571182355221987,4.67090374066804));
#8486=CARTESIAN_POINT('Ctrl Pts',(6.52274298444712,-0.241477409664008,4.49049679612232));
#8487=CARTESIAN_POINT('Ctrl Pts',(6.53349756884893,0.0501147882500171,4.46748118948392));
#8488=CARTESIAN_POINT('Ctrl Pts',(6.54155389312568,0.265195219859689,4.51115221205005));
#8489=CARTESIAN_POINT('Ctrl Pts',(6.54965647563047,0.459973714137355,4.6129814833824));
#8490=CARTESIAN_POINT('Ctrl Pts',(6.5576758012139,0.619037348482741,4.76486078836297));
#8491=CARTESIAN_POINT('Ctrl Pts',(6.5638565028091,0.702214918141095,4.90753456196431));
#8492=CARTESIAN_POINT('Ctrl Pts',(6.56774522291797,0.739840261363108,5.01001808408939));
#8493=CARTESIAN_POINT('Ctrl Pts',(6.56982725311109,0.755173986750213,5.06276611003264));
#8494=CARTESIAN_POINT('Ctrl Pts',(6.57223182121529,0.766523132772943,5.11606099522602));
#8495=CARTESIAN_POINT('Ctrl Pts',(6.57393262316656,0.776748482011025,5.18626717050706));
#8496=CARTESIAN_POINT('Ctrl Pts',(6.57802798038273,0.780117929748685,5.28278909253043));
#8497=CARTESIAN_POINT('Ctrl Pts',(6.59124494998433,0.764983429094594,5.42671920642507));
#8498=CARTESIAN_POINT('Ctrl Pts',(6.60956554315219,0.68572326715126,5.67210008102203));
#8499=CARTESIAN_POINT('Ctrl Pts',(6.63342570307357,0.482275698626895,5.89729441612607));
#8500=CARTESIAN_POINT('Ctrl Pts',(6.65569976703258,0.211186373881766,6.01644845156957));
#8501=CARTESIAN_POINT('Ctrl Pts',(6.67857023173211,-0.0824821450646381,
6.05674685227899));
#8502=CARTESIAN_POINT('Ctrl Pts',(6.70693191311676,-0.449782403728053,5.94930974724307));
#8503=CARTESIAN_POINT('Ctrl Pts',(6.74000644362055,-0.743697403464958,5.61692476045587));
#8504=CARTESIAN_POINT('Ctrl Pts',(6.77183780370126,-0.825660357870783,5.20051970189362));
#8505=CARTESIAN_POINT('Ctrl Pts',(6.80251278275663,-0.703475060709293,4.81085211691783));
#8506=CARTESIAN_POINT('Ctrl Pts',(6.83325307834601,-0.409020216329708,4.52616875178095));
#8507=CARTESIAN_POINT('Ctrl Pts',(6.86407778139747,-0.013438207806227,4.41681026053004));
#8508=CARTESIAN_POINT('Ctrl Pts',(6.89496847918126,0.387190546300914,4.50998959025875));
#8509=CARTESIAN_POINT('Ctrl Pts',(6.92334526410876,0.669439165256199,4.76162282320026));
#8510=CARTESIAN_POINT('Ctrl Pts',(6.94918439495235,0.803100128876369,5.07308158460193));
#8511=CARTESIAN_POINT('Ctrl Pts',(6.98023347108384,0.818138478146011,5.48132682598222));
#8512=CARTESIAN_POINT('Ctrl Pts',(7.01393507577349,0.583765048880111,5.88323952969222));
#8513=CARTESIAN_POINT('Ctrl Pts',(7.05029034196779,0.140714106057853,6.08003730568266));
#8514=CARTESIAN_POINT('Ctrl Pts',(7.08149210594045,-0.273016084884725,6.04746437682534));
#8515=CARTESIAN_POINT('Ctrl Pts',(7.10622343068897,-0.549029305695015,5.86769627218021));
#8516=CARTESIAN_POINT('Ctrl Pts',(7.1244552483263,-0.692090135230285,5.67952629490147));
#8517=CARTESIAN_POINT('Ctrl Pts',(7.14008798549728,-0.782618105115043,5.49838936905692));
#8518=CARTESIAN_POINT('Ctrl Pts',(7.16745761696029,-0.849577897570751,5.14473853593693));
#8519=CARTESIAN_POINT('Ctrl Pts',(7.20658941040099,-0.650684341966546,4.64158371398262));
#8520=CARTESIAN_POINT('Ctrl Pts',(7.25357695572029,-0.0633045461604468,
4.3609623615544));
#8521=CARTESIAN_POINT('Ctrl Pts',(7.30057733164244,0.557708033944997,4.55491612196963));
#8522=CARTESIAN_POINT('Ctrl Pts',(7.34757286249331,0.881406337177324,5.11912513726633));
#8523=CARTESIAN_POINT('Ctrl Pts',(7.39454538146955,0.734686256930202,5.75319528327261));
#8524=CARTESIAN_POINT('Ctrl Pts',(7.43365687136522,0.286617000227074,6.05598265751437));
#8525=CARTESIAN_POINT('Ctrl Pts',(7.46491538644837,-0.124078879570498,6.06888030729612));
#8526=CARTESIAN_POINT('Ctrl Pts',(7.49094515362771,-0.446422101358953,5.95583388766042));
#8527=CARTESIAN_POINT('Ctrl Pts',(7.51955536822179,-0.718525845560669,5.68904753107812));
#8528=CARTESIAN_POINT('Ctrl Pts',(7.55072731520184,-0.839977697613594,5.29213009146162));
#8529=CARTESIAN_POINT('Ctrl Pts',(7.57666686463738,-0.770445104836072,4.95383991243434));
#8530=CARTESIAN_POINT('Ctrl Pts',(7.59739316080166,-0.623484139109556,4.7278712732606));
#8531=CARTESIAN_POINT('Ctrl Pts',(7.61810309328136,-0.425660210814252,4.54466649182984));
#8532=CARTESIAN_POINT('Ctrl Pts',(7.64396055049064,-0.105529779735548,4.4199311002941));
#8533=CARTESIAN_POINT('Ctrl Pts',(7.68008681845853,0.372701727578117,4.47952100368038));
#8534=CARTESIAN_POINT('Ctrl Pts',(7.71355248212602,0.710651761559828,4.79483205441596));
#8535=CARTESIAN_POINT('Ctrl Pts',(7.7443629084714,0.812996711285813,5.18686102863723));
#8536=CARTESIAN_POINT('Ctrl Pts',(7.77512035944637,0.768988465478849,5.58810403940493));
#8537=CARTESIAN_POINT('Ctrl Pts',(7.81346225286718,0.437720151424322,6.00298785716469));
#8538=CARTESIAN_POINT('Ctrl Pts',(7.85546711372016,-0.137253206275788,6.08763408005374));
#8539=CARTESIAN_POINT('Ctrl Pts',(7.89350847994605,-0.583738633090295,5.83892102537973));
#8540=CARTESIAN_POINT('Ctrl Pts',(7.92763049904828,-0.804821403375952,5.43809078417017));
#8541=CARTESIAN_POINT('Ctrl Pts',(7.9531308415908,-0.785069701277599,5.09628801507745));
#8542=CARTESIAN_POINT('Ctrl Pts',(7.97008865655783,-0.697928181014753,4.89491411877532));
#8543=CARTESIAN_POINT('Ctrl Pts',(7.97855948171228,-0.640915735564249,4.80135284223213));
#8544=CARTESIAN_POINT('Ctrl Pts',(7.98702215880035,-0.571366863372613,4.71669331991059));
#8545=CARTESIAN_POINT('Ctrl Pts',(8.00017374436506,-0.446089544766635,4.60185560278705));
#8546=CARTESIAN_POINT('Ctrl Pts',(8.02549283150456,-0.151845066061863,4.44472298246148));
#8547=CARTESIAN_POINT('Ctrl Pts',(8.05911401414102,0.310851653233882,4.4803431473172));
#8548=CARTESIAN_POINT('Ctrl Pts',(8.09628982312233,0.682960272889444,4.81493413878844));
#8549=CARTESIAN_POINT('Ctrl Pts',(8.12960374965605,0.806389045514395,5.24399675485307));
#8550=CARTESIAN_POINT('Ctrl Pts',(8.16276733565534,0.682922920155554,5.67208701553495));
#8551=CARTESIAN_POINT('Ctrl Pts',(8.19577818693008,0.352311944327571,5.9670837080692));
#8552=CARTESIAN_POINT('Ctrl Pts',(8.22863264240994,-0.0825629153572059,
6.04087783376966));
#8553=CARTESIAN_POINT('Ctrl Pts',(8.26132800369485,-0.488067210769859,5.87276577273915));
#8554=CARTESIAN_POINT('Ctrl Pts',(8.29386155280421,-0.74077637673532,5.51652145653297));
#8555=CARTESIAN_POINT('Ctrl Pts',(8.3262310099455,-0.765141573786744,5.08261410411509));
#8556=CARTESIAN_POINT('Ctrl Pts',(8.35843433417891,-0.556044846512561,4.70418551870374));
#8557=CARTESIAN_POINT('Ctrl Pts',(8.39046982367808,-0.179657347321662,4.49604889689588));
#8558=CARTESIAN_POINT('Ctrl Pts',(8.42233607195163,0.247511742503061,4.5198871077102));
#8559=CARTESIAN_POINT('Ctrl Pts',(8.45403200084779,0.594683503231845,4.76597769364031));
#8560=CARTESIAN_POINT('Ctrl Pts',(8.48555684223994,0.756894001188261,5.15690766378376));
#8561=CARTESIAN_POINT('Ctrl Pts',(8.51691015446463,0.68666220127433,5.57197297916182));
#8562=CARTESIAN_POINT('Ctrl Pts',(8.54809180995931,0.407998968484439,5.88433263611551));
#8563=CARTESIAN_POINT('Ctrl Pts',(8.57910201533282,0.00795162764025913,
6.00004580282724));
#8564=CARTESIAN_POINT('Ctrl Pts',(8.6048013940002,-0.323544528379635,5.90474031577638));
#8565=CARTESIAN_POINT('Ctrl Pts',(8.62527588995087,-0.527538523543061,5.73261036130886));
#8566=CARTESIAN_POINT('Ctrl Pts',(8.64455963194646,-0.667794018511264,5.52405322458113));
#8567=CARTESIAN_POINT('Ctrl Pts',(8.66772398150025,-0.729516788746334,5.22178980165561));
#8568=CARTESIAN_POINT('Ctrl Pts',(8.6947115213019,-0.623992833684527,4.87839995894372));
#8569=CARTESIAN_POINT('Ctrl Pts',(8.71932941129584,-0.389778889903979,4.64889155370676));
#8570=CARTESIAN_POINT('Ctrl Pts',(8.74161491094236,-0.113760951060223,4.55235377325117));
#8571=CARTESIAN_POINT('Ctrl Pts',(8.76826131811639,0.236463642093971,4.56332162481603));
#8572=CARTESIAN_POINT('Ctrl Pts',(8.8013895184305,0.615841184389589,4.82017769980994));
#8573=CARTESIAN_POINT('Ctrl Pts',(8.84086340331569,0.738210427752782,5.35350219278022));
#8574=CARTESIAN_POINT('Ctrl Pts',(8.88006472675475,0.46774700707792,5.82374541850904));
#8575=CARTESIAN_POINT('Ctrl Pts',(8.9190021131565,-0.0473547807328733,5.9839561652154));
#8576=CARTESIAN_POINT('Ctrl Pts',(8.95123692710172,-0.449393545951968,5.79074568682316));
#8577=CARTESIAN_POINT('Ctrl Pts',(8.97690325278144,-0.628299851082753,5.50527526375753));
#8578=CARTESIAN_POINT('Ctrl Pts',(9.00249067541009,-0.69348799230158,5.17511262738361));
#8579=CARTESIAN_POINT('Ctrl Pts',(9.0300818610813,-0.555353587350565,4.81986222419062));
#8580=CARTESIAN_POINT('Ctrl Pts',(9.0596537824972,-0.224198845203747,4.60565111673752));
#8581=CARTESIAN_POINT('Ctrl Pts',(9.08490549546368,0.110568591021175,4.57910492629159));
#8582=CARTESIAN_POINT('Ctrl Pts',(9.11111456267047,0.429517962801524,4.72156968021327));
#8583=CARTESIAN_POINT('Ctrl Pts',(9.13826748581402,0.641572051369251,5.01801495571582));
#8584=CARTESIAN_POINT('Ctrl Pts',(9.16636064343759,0.664243389357046,5.39466135553552));
#8585=CARTESIAN_POINT('Ctrl Pts',(9.19435473755382,0.483712991221918,5.72436734483168));
#8586=CARTESIAN_POINT('Ctrl Pts',(9.22225428967748,0.156556617497767,5.90697725081521));
#8587=CARTESIAN_POINT('Ctrl Pts',(9.25006860981886,-0.216462968184482,5.88762228369914));
#8588=CARTESIAN_POINT('Ctrl Pts',(9.27779490424495,-0.521173298004424,5.67345613827036));
#8589=CARTESIAN_POINT('Ctrl Pts',(9.30545764377868,-0.664905802214252,5.33089556329931));
#8590=CARTESIAN_POINT('Ctrl Pts',(9.33301923890341,-0.604574180753094,4.96529698499221));
#8591=CARTESIAN_POINT('Ctrl Pts',(9.36057937654899,-0.359512498236151,4.68826678446829));
#8592=CARTESIAN_POINT('Ctrl Pts',(9.38336763883071,-0.0644150007369484,
4.60181005320466));
#8593=CARTESIAN_POINT('Ctrl Pts',(9.40177229277858,0.171957864695282,4.63424204726826));
#8594=CARTESIAN_POINT('Ctrl Pts',(9.41971547820392,0.390339392509962,4.73014944693566));
#8595=CARTESIAN_POINT('Ctrl Pts',(9.43896126596102,0.554595856232393,4.91197438114008));
#8596=CARTESIAN_POINT('Ctrl Pts',(9.45378482555719,0.618730996160634,5.11023167780338));
#8597=CARTESIAN_POINT('Ctrl Pts',(9.46450812670568,0.630993754219246,5.22742155461715));
#8598=CARTESIAN_POINT('Ctrl Pts',(9.46764503127636,0.628297080576472,5.30219028275335));
#8599=CARTESIAN_POINT('Ctrl Pts',(9.46908405130908,0.619988284606207,5.36019955318967));
#8600=CARTESIAN_POINT('Ctrl Pts',(9.47102628349308,0.610719630094374,5.40339518180637));
#8601=CARTESIAN_POINT('Ctrl Pts',(9.47270676110673,0.598391365633221,5.44590610393438));
#8602=CARTESIAN_POINT('Ctrl Pts',(9.47585389932824,0.567911563922736,5.52888863921652));
#8603=CARTESIAN_POINT('Ctrl Pts',(9.48086157752316,0.500540513684368,5.6444944560202));
#8604=CARTESIAN_POINT('Ctrl Pts',(9.4873632826241,0.371548176565824,5.76766631765112));
#8605=CARTESIAN_POINT('Ctrl Pts',(9.49393826309572,0.213479131284237,5.85031521547837));
#8606=CARTESIAN_POINT('Ctrl Pts',(9.5004811182654,0.0387777611901389,5.88579913080903));
#8607=CARTESIAN_POINT('Ctrl Pts',(9.50922333920638,-0.198282351728511,5.86709693896304));
#8608=CARTESIAN_POINT('Ctrl Pts',(9.52013452774334,-0.46667830079645,5.72032868888011));
#8609=CARTESIAN_POINT('Ctrl Pts',(9.53323680753399,-0.645398555208325,5.39939701305271));
#8610=CARTESIAN_POINT('Ctrl Pts',(9.54633608057676,-0.625836293082998,5.03285670636973));
#8611=CARTESIAN_POINT('Ctrl Pts',(9.55943542919992,-0.414150298918583,4.73277350781654));
#8612=CARTESIAN_POINT('Ctrl Pts',(9.57253867700424,-0.0751472013293622,
4.59190807185631));
#8613=CARTESIAN_POINT('Ctrl Pts',(9.58564225817841,0.286850803022957,4.65267462198366));
#8614=CARTESIAN_POINT('Ctrl Pts',(9.59875166752506,0.560859734073248,4.89747222799095));
#8615=CARTESIAN_POINT('Ctrl Pts',(9.6074850747912,0.628637838448434,5.13210373452291));
#8616=CARTESIAN_POINT('Ctrl Pts',(9.61186183958885,0.628653751959821,5.25031361552224));
#8617=CARTESIAN_POINT('Ctrl Pts',(6.39751711228746,0.680624720495572,5.25304865882655));
#8618=CARTESIAN_POINT('Ctrl Pts',(6.40225233315809,0.680607503670563,5.38093990420756));
#8619=CARTESIAN_POINT('Ctrl Pts',(6.41172205109112,0.607201745611839,5.63535890108503));
#8620=CARTESIAN_POINT('Ctrl Pts',(6.4259709706028,0.309516653578047,5.90146181902454));
#8621=CARTESIAN_POINT('Ctrl Pts',(6.44025312148205,-0.0850383123659948,
5.96797084256395));
#8622=CARTESIAN_POINT('Ctrl Pts',(6.45457324150139,-0.455365964413035,5.81391716320603));
#8623=CARTESIAN_POINT('Ctrl Pts',(6.46892916984286,-0.687635090018441,5.48549609831644));
#8624=CARTESIAN_POINT('Ctrl Pts',(6.48331906612102,-0.709165727198881,5.08280191239329));
#8625=CARTESIAN_POINT('Ctrl Pts',(6.49774922577713,-0.512546421676701,4.72939501254341));
#8626=CARTESIAN_POINT('Ctrl Pts',(6.50979652059476,-0.216309306596918,4.56725927170696));
#8627=CARTESIAN_POINT('Ctrl Pts',(6.51946444783249,0.0458261865225807,4.54656004710209));
#8628=CARTESIAN_POINT('Ctrl Pts',(6.52670907638838,0.239239492269565,4.58582571736047));
#8629=CARTESIAN_POINT('Ctrl Pts',(6.53399753413874,0.414459889663216,4.67742201785098));
#8630=CARTESIAN_POINT('Ctrl Pts',(6.54121399209174,0.557593347876044,4.81408955941056));
#8631=CARTESIAN_POINT('Ctrl Pts',(6.54677694631745,0.632480164682304,4.94251960028035));
#8632=CARTESIAN_POINT('Ctrl Pts',(6.55027966996043,0.666354521129582,5.03480968054718));
#8633=CARTESIAN_POINT('Ctrl Pts',(6.55215763463341,0.68021361955907,5.08242581586253));
#8634=CARTESIAN_POINT('Ctrl Pts',(6.55432583571746,0.690388365771941,5.13039821778687));
#8635=CARTESIAN_POINT('Ctrl Pts',(6.5558212094319,0.699578648143096,5.19293901702375));
#8636=CARTESIAN_POINT('Ctrl Pts',(6.55961298540583,0.702633425884744,5.28183421164039));
#8637=CARTESIAN_POINT('Ctrl Pts',(6.57151606473466,0.68899661596649,5.41123234210713));
#8638=CARTESIAN_POINT('Ctrl Pts',(6.58803656661797,0.617521153603729,5.63265929180953));
#8639=CARTESIAN_POINT('Ctrl Pts',(6.60958516286006,0.433851269549472,5.83600755874635));
#8640=CARTESIAN_POINT('Ctrl Pts',(6.62973248808607,0.188640588438607,5.94384063293095));
#8641=CARTESIAN_POINT('Ctrl Pts',(6.65043835762877,-0.0772361906896132,
5.98033717006274));
#8642=CARTESIAN_POINT('Ctrl Pts',(6.67615394337537,-0.410324683989954,5.88303784137002));
#8643=CARTESIAN_POINT('Ctrl Pts',(6.70620834369982,-0.677527627921871,5.58106727717635));
#8644=CARTESIAN_POINT('Ctrl Pts',(6.73519774391456,-0.752289167263662,5.20183502623849));
#8645=CARTESIAN_POINT('Ctrl Pts',(6.76319532038265,-0.64086301682906,4.84611638250373));
#8646=CARTESIAN_POINT('Ctrl Pts',(6.79131667826662,-0.371548691224543,4.58557649574375));
#8647=CARTESIAN_POINT('Ctrl Pts',(6.81958651831909,-0.00876747492102148,
4.48516204186951));
#8648=CARTESIAN_POINT('Ctrl Pts',(6.84798778593148,0.359625721045227,4.57071606330109));
#8649=CARTESIAN_POINT('Ctrl Pts',(6.87414419186486,0.619911226291208,4.80259762964785));
#8650=CARTESIAN_POINT('Ctrl Pts',(6.89802078290191,0.743479804719753,5.09040348007126));
#8651=CARTESIAN_POINT('Ctrl Pts',(6.92677090249117,0.75749740723106,5.46842641189442));
#8652=CARTESIAN_POINT('Ctrl Pts',(6.9580730057421,0.540057022180745,5.84196132934458));
#8653=CARTESIAN_POINT('Ctrl Pts',(6.99197236356748,0.126976780802123,6.02565755911728));
#8654=CARTESIAN_POINT('Ctrl Pts',(7.02115368307822,-0.260018076161804,5.99532829292384));
#8655=CARTESIAN_POINT('Ctrl Pts',(7.04435146484917,-0.51904605885336,5.82677537589849));
#8656=CARTESIAN_POINT('Ctrl Pts',(7.06149524329004,-0.653591100025065,5.64982744492753));
#8657=CARTESIAN_POINT('Ctrl Pts',(7.07621223459031,-0.738832249764652,5.47928733188006));
#8658=CARTESIAN_POINT('Ctrl Pts',(7.10202582573893,-0.802074067065736,5.14575072437161));
#8659=CARTESIAN_POINT('Ctrl Pts',(7.1390661714286,-0.614219467641983,4.66923696198742));
#8660=CARTESIAN_POINT('Ctrl Pts',(7.1837708745735,-0.0555595921669689,4.40165548662197));
#8661=CARTESIAN_POINT('Ctrl Pts',(7.22872116331736,0.538653928108292,4.58659194717158));
#8662=CARTESIAN_POINT('Ctrl Pts',(7.27390617378398,0.850481830515366,5.12883749998695));
#8663=CARTESIAN_POINT('Ctrl Pts',(7.31931488180511,0.709264792487632,5.74204700545256));
#8664=CARTESIAN_POINT('Ctrl Pts',(7.35733020712546,0.273950364552491,6.0368560795042));
#8665=CARTESIAN_POINT('Ctrl Pts',(7.38784321768943,-0.127026135903747,6.04956111280713));
#8666=CARTESIAN_POINT('Ctrl Pts',(7.41332435274361,-0.442622948923682,5.93897098677174));
#8667=CARTESIAN_POINT('Ctrl Pts',(7.44141540477827,-0.709991267168369,5.67708175603403));
#8668=CARTESIAN_POINT('Ctrl Pts',(7.47213867876536,-0.829919462138918,5.2858425046348));
#8669=CARTESIAN_POINT('Ctrl Pts',(7.49780365676607,-0.761260797305466,4.9510296020902));
#8670=CARTESIAN_POINT('Ctrl Pts',(7.51837138045615,-0.615435449184283,4.72674446363352));
#8671=CARTESIAN_POINT('Ctrl Pts',(7.53896082495651,-0.41876479320792,4.54455336747707));
#8672=CARTESIAN_POINT('Ctrl Pts',(7.56473451809807,-0.0996332587151797,
4.42005806517321));
#8673=CARTESIAN_POINT('Ctrl Pts',(7.60089474682253,0.379071768057273,4.47943617181632));
#8674=CARTESIAN_POINT('Ctrl Pts',(7.63454183470689,0.719245239568688,4.79620324937939));
#8675=CARTESIAN_POINT('Ctrl Pts',(7.66565790477818,0.822745840976506,5.19215366233993));
#8676=CARTESIAN_POINT('Ctrl Pts',(7.69680539567309,0.778276356479982,5.59852018046501));
#8677=CARTESIAN_POINT('Ctrl Pts',(7.73579429186146,0.441792674687113,6.02084310589315));
#8678=CARTESIAN_POINT('Ctrl Pts',(7.77875200546607,-0.146245218710824,6.10803158972312));
#8679=CARTESIAN_POINT('Ctrl Pts',(7.81784579628705,-0.60534328507275,5.85266747212583));
#8680=CARTESIAN_POINT('Ctrl Pts',(7.85305201517912,-0.833732751184462,5.43911762567102));
#8681=CARTESIAN_POINT('Ctrl Pts',(7.87946834695168,-0.813465377269389,5.08491801220921));
#8682=CARTESIAN_POINT('Ctrl Pts',(7.89708605095421,-0.722929329258105,4.87568490176684));
#8683=CARTESIAN_POINT('Ctrl Pts',(7.90589543440468,-0.663637678579888,4.77837755008365));
#8684=CARTESIAN_POINT('Ctrl Pts',(7.9147052348979,-0.591235696995094,4.69023621557549));
#8685=CARTESIAN_POINT('Ctrl Pts',(7.92840949236335,-0.460683037030015,4.57056164963325));
#8686=CARTESIAN_POINT('Ctrl Pts',(7.95483860408169,-0.15358027728359,4.40642966995394));
#8687=CARTESIAN_POINT('Ctrl Pts',(7.9900782106196,0.331443518324377,4.44333298030211));
#8688=CARTESIAN_POINT('Ctrl Pts',(8.02921328460596,0.723445785656926,4.7953838211401));
#8689=CARTESIAN_POINT('Ctrl Pts',(8.06441280659302,0.854101409558101,5.24877038721031));
#8690=CARTESIAN_POINT('Ctrl Pts',(8.09958701599841,0.723363692643256,5.70295040335949));
#8691=CARTESIAN_POINT('Ctrl Pts',(8.13472653743285,0.371518171835058,6.01720091545639));
#8692=CARTESIAN_POINT('Ctrl Pts',(8.16982494145643,-0.0930948557614484,
6.09627059007613));
#8693=CARTESIAN_POINT('Ctrl Pts',(8.20487462262262,-0.527954026710614,5.91623039165312));
#8694=CARTESIAN_POINT('Ctrl Pts',(8.23986864821332,-0.799991604059477,5.53311237459394));
#8695=CARTESIAN_POINT('Ctrl Pts',(8.27479996206171,-0.826498178537887,5.0648109106924));
#8696=CARTESIAN_POINT('Ctrl Pts',(8.30966173141794,-0.600287084615231,4.65499186138042));
#8697=CARTESIAN_POINT('Ctrl Pts',(8.34444722908088,-0.191633025309102,4.4287921691465));
#8698=CARTESIAN_POINT('Ctrl Pts',(8.37914985495973,0.273621969842747,4.45457183677348));
#8699=CARTESIAN_POINT('Ctrl Pts',(8.41376322201856,0.652891126786519,4.72320094977889));
#8700=CARTESIAN_POINT('Ctrl Pts',(8.44828100386036,0.830672841389853,5.1512269951916));
#8701=CARTESIAN_POINT('Ctrl Pts',(8.48269725010349,0.753725327560749,5.60691060360366));
#8702=CARTESIAN_POINT('Ctrl Pts',(8.51700574767951,0.447197440440791,5.95072247183271));
#8703=CARTESIAN_POINT('Ctrl Pts',(8.55120147675044,0.006056982700166,6.07846248484495));
#8704=CARTESIAN_POINT('Ctrl Pts',(8.5795979930875,-0.360294905244475,5.97323947341581));
#8705=CARTESIAN_POINT('Ctrl Pts',(8.60225515093291,-0.586058809991556,5.78276387703451));
#8706=CARTESIAN_POINT('Ctrl Pts',(8.62361400547052,-0.741423193618978,5.55176886084562));
#8707=CARTESIAN_POINT('Ctrl Pts',(8.6492993869632,-0.80992882190433,5.21659456869169));
#8708=CARTESIAN_POINT('Ctrl Pts',(8.67926816021605,-0.692803381724077,4.83524213198653));
#8709=CARTESIAN_POINT('Ctrl Pts',(8.70663907035742,-0.432425467034378,4.58002223923859));
#8710=CARTESIAN_POINT('Ctrl Pts',(8.73144096068225,-0.125235700856212,4.47256383401499));
#8711=CARTESIAN_POINT('Ctrl Pts',(8.76111878191403,0.264829760437898,4.48474922697656));
#8712=CARTESIAN_POINT('Ctrl Pts',(8.7980518821071,0.687841587709185,4.77102417277571));
#8713=CARTESIAN_POINT('Ctrl Pts',(8.84210282382596,0.824487236093128,5.36617546269049));
#8714=CARTESIAN_POINT('Ctrl Pts',(8.88587709935538,0.522509612312472,5.8912941405695));
#8715=CARTESIAN_POINT('Ctrl Pts',(8.92936793745018,-0.0528251778134879,
6.07023871034585));
#8716=CARTESIAN_POINT('Ctrl Pts',(8.96536876448126,-0.501804297185836,5.85442740754525));
#8717=CARTESIAN_POINT('Ctrl Pts',(8.9940226207963,-0.701513395856217,5.53573257462399));
#8718=CARTESIAN_POINT('Ctrl Pts',(9.02257790961678,-0.774248572961943,5.16726969518564));
#8719=CARTESIAN_POINT('Ctrl Pts',(9.05335063398794,-0.620113902972228,4.77110979993558));
#8720=CARTESIAN_POINT('Ctrl Pts',(9.08629550322002,-0.251166130286266,4.53251972549975));
#8721=CARTESIAN_POINT('Ctrl Pts',(9.11439923362155,0.121398725300332,4.50302942635595));
#8722=CARTESIAN_POINT('Ctrl Pts',(9.14353314968954,0.475903959542619,4.66144572731908));
#8723=CARTESIAN_POINT('Ctrl Pts',(9.17367583697776,0.711198057444889,4.99054851242612));
#8724=CARTESIAN_POINT('Ctrl Pts',(9.20480613272535,0.73620666788718,5.40787508252366));
#8725=CARTESIAN_POINT('Ctrl Pts',(9.23576528071196,0.536473915806161,5.77239779939988));
#8726=CARTESIAN_POINT('Ctrl Pts',(9.2665517671634,0.175449514853214,5.97375916418192));
#8727=CARTESIAN_POINT('Ctrl Pts',(9.29716995899978,-0.235102434914403,5.95230969541478));
#8728=CARTESIAN_POINT('Ctrl Pts',(9.32761122417275,-0.569496724483142,5.71708404420856));
#8729=CARTESIAN_POINT('Ctrl Pts',(9.3578961346874,-0.726661568437755,5.3420504815634));
#8730=CARTESIAN_POINT('Ctrl Pts',(9.3879795972285,-0.660627831242916,4.9431304051231));
#8731=CARTESIAN_POINT('Ctrl Pts',(9.41796225151563,-0.393914336295686,4.64193363228604));
#8732=CARTESIAN_POINT('Ctrl Pts',(9.44267196720143,-0.0739628444132731,
4.5484248269869));
#8733=CARTESIAN_POINT('Ctrl Pts',(9.46256871425264,0.181534913420138,4.58349805707381));
#8734=CARTESIAN_POINT('Ctrl Pts',(9.48193099055251,0.417177415012966,4.68711079083017));
#8735=CARTESIAN_POINT('Ctrl Pts',(9.50264761041058,0.59376362870692,4.8826065496897));
#8736=CARTESIAN_POINT('Ctrl Pts',(9.51853337553614,0.662492027814835,5.09547907660583));
#8737=CARTESIAN_POINT('Ctrl Pts',(9.52998397381837,0.675608484942566,5.22002390776071));
#8738=CARTESIAN_POINT('Ctrl Pts',(9.53360187787314,0.672675837184915,5.30497027631959));
#8739=CARTESIAN_POINT('Ctrl Pts',(9.5350497840785,0.663833420845446,5.3652973078514));
#8740=CARTESIAN_POINT('Ctrl Pts',(9.5371341248435,0.6540363023188,5.41143656975418));
#8741=CARTESIAN_POINT('Ctrl Pts',(9.53893927072564,0.640722782477816,5.45719451112064));
#8742=CARTESIAN_POINT('Ctrl Pts',(9.54230746605352,0.608145268610779,5.54594483650046));
#8743=CARTESIAN_POINT('Ctrl Pts',(9.54765843321268,0.536123532477182,5.66946706886201));
#8744=CARTESIAN_POINT('Ctrl Pts',(9.55460011238389,0.398445319464292,5.8009270775643));
#8745=CARTESIAN_POINT('Ctrl Pts',(9.56161210819828,0.229883573084278,5.88904451423784));
#8746=CARTESIAN_POINT('Ctrl Pts',(9.56858274424492,0.0437972897715726,5.92682689027164));
#8747=CARTESIAN_POINT('Ctrl Pts',(9.57788611107426,-0.208446314292508,5.90690665257042));
#8748=CARTESIAN_POINT('Ctrl Pts',(9.58948273544246,-0.493550672467801,5.75088826678903));
#8749=CARTESIAN_POINT('Ctrl Pts',(9.60337628935687,-0.682895977604234,5.41060732952618));
#8750=CARTESIAN_POINT('Ctrl Pts',(9.61723630723951,-0.662079175861379,5.02289243557709));
#8751=CARTESIAN_POINT('Ctrl Pts',(9.63106693440455,-0.438529006711427,4.70624313314514));
#8752=CARTESIAN_POINT('Ctrl Pts',(9.64486774996197,-0.0814919091113444,
4.55801911650286));
#8753=CARTESIAN_POINT('Ctrl Pts',(9.65863703887208,0.298830266437039,4.62199877125373));
#8754=CARTESIAN_POINT('Ctrl Pts',(9.67238031930236,0.585981516491704,4.87868849034264));
#8755=CARTESIAN_POINT('Ctrl Pts',(9.68151652791651,0.656819784319085,5.12410843764133));
#8756=CARTESIAN_POINT('Ctrl Pts',(9.68608742684445,0.656836403684187,5.24756159158325));
#8757=CARTESIAN_POINT('Ctrl Pts',(6.45926094481572,0.630631645298518,5.25075584038089));
#8758=CARTESIAN_POINT('Ctrl Pts',(6.46365212293046,0.63061567938114,5.36935500462839));
#8759=CARTESIAN_POINT('Ctrl Pts',(6.47241635726032,0.562620260489693,5.60485419658667));
#8760=CARTESIAN_POINT('Ctrl Pts',(6.48558625248065,0.287416865857649,5.85077154136491));
#8761=CARTESIAN_POINT('Ctrl Pts',(6.49876139799279,-0.0766327666807152,
5.91202548479231));
#8762=CARTESIAN_POINT('Ctrl Pts',(6.51195067642553,-0.417708947598931,5.77004045811818));
#8763=CARTESIAN_POINT('Ctrl Pts',(6.52514978293253,-0.631222811810323,5.46797327754339));
#8764=CARTESIAN_POINT('Ctrl Pts',(6.53835654602454,-0.650891881237755,5.09827400825114));
#8765=CARTESIAN_POINT('Ctrl Pts',(6.55158109914582,-0.470586715770342,4.77436995516259));
#8766=CARTESIAN_POINT('Ctrl Pts',(6.56260333534973,-0.199433661178286,4.62604524416983));
#8767=CARTESIAN_POINT('Ctrl Pts',(6.571441254142,0.0402205362572792,4.60713511034868));
#8768=CARTESIAN_POINT('Ctrl Pts',(6.57805870994194,0.216917555899971,4.64301726701627));
#8769=CARTESIAN_POINT('Ctrl Pts',(6.58471156897691,0.376868484589112,4.7266438859889));
#8770=CARTESIAN_POINT('Ctrl Pts',(6.59129368162691,0.507448482818788,4.8513301406675));
#8771=CARTESIAN_POINT('Ctrl Pts',(6.59636476168569,0.575693818909383,4.96841258612528));
#8772=CARTESIAN_POINT('Ctrl Pts',(6.59955449451534,0.606568241636653,5.05249416408791));
#8773=CARTESIAN_POINT('Ctrl Pts',(6.60126044558016,0.619113836374534,5.09569120029176));
#8774=CARTESIAN_POINT('Ctrl Pts',(6.60323132681257,0.628456403477267,5.13943435527507));
#8775=CARTESIAN_POINT('Ctrl Pts',(6.6046510101575,0.636856623460891,5.19748854771694));
#8776=CARTESIAN_POINT('Ctrl Pts',(6.6079401285395,0.639609543705504,5.27534803811019));
#8777=CARTESIAN_POINT('Ctrl Pts',(6.61879883010074,0.627183581911554,5.39376860016358));
#8778=CARTESIAN_POINT('Ctrl Pts',(6.63383329382943,0.562134630004875,5.59501981359328));
#8779=CARTESIAN_POINT('Ctrl Pts',(6.65338763271038,0.395327976071264,5.77969125230577));
#8780=CARTESIAN_POINT('Ctrl Pts',(6.67164286743441,0.173140595239862,5.87732250405325));
#8781=CARTESIAN_POINT('Ctrl Pts',(6.69038342521688,-0.0675226512948717,
5.91034880637455));
#8782=CARTESIAN_POINT('Ctrl Pts',(6.71361724126403,-0.368479602326163,5.82230340539203));
#8783=CARTESIAN_POINT('Ctrl Pts',(6.74072150009791,-0.60939880453155,5.54988058932266));
#8784=CARTESIAN_POINT('Ctrl Pts',(6.76682335000588,-0.676647905208886,5.2083655360096));
#8785=CARTESIAN_POINT('Ctrl Pts',(6.79199917821714,-0.576386826274553,4.88848696990566));
#8786=CARTESIAN_POINT('Ctrl Pts',(6.81725659668747,-0.334439787297777,4.65449398609593));
#8787=CARTESIAN_POINT('Ctrl Pts',(6.84262441363562,-0.00888238488552531,
4.56442303985172));
#8788=CARTESIAN_POINT('Ctrl Pts',(6.86808919715576,0.321423032235318,4.64116571674426));
#8789=CARTESIAN_POINT('Ctrl Pts',(6.89152618201979,0.554634130589795,4.84896006600901));
#8790=CARTESIAN_POINT('Ctrl Pts',(6.91291206541523,0.665305615860708,5.10674832578124));
#8791=CARTESIAN_POINT('Ctrl Pts',(6.93865672617456,0.677845262595485,5.44525276052196));
#8792=CARTESIAN_POINT('Ctrl Pts',(6.9666802969137,0.483167022914325,5.77965370335718));
#8793=CARTESIAN_POINT('Ctrl Pts',(6.99703059331053,0.113343713819975,5.94411784378224));
#8794=CARTESIAN_POINT('Ctrl Pts',(7.0231623426855,-0.23320446349144,5.91696869874648));
#8795=CARTESIAN_POINT('Ctrl Pts',(7.04394514044647,-0.465252901929868,5.76598107103288));
#8796=CARTESIAN_POINT('Ctrl Pts',(7.05930843146434,-0.585824133571807,5.60741425568615));
#8797=CARTESIAN_POINT('Ctrl Pts',(7.07250016431883,-0.66222795488503,5.45455360274052));
#8798=CARTESIAN_POINT('Ctrl Pts',(7.09564685442722,-0.718945508527952,5.15549592008938));
#8799=CARTESIAN_POINT('Ctrl Pts',(7.12889075561355,-0.550454960488801,4.72782148892568));
#8800=CARTESIAN_POINT('Ctrl Pts',(7.16907295422903,-0.0484319759876638,
4.48718062663814));
#8801=CARTESIAN_POINT('Ctrl Pts',(7.20954974681085,0.486652722950244,4.65350202049014));
#8802=CARTESIAN_POINT('Ctrl Pts',(7.25032543086917,0.768219032236227,5.14265428374656));
#8803=CARTESIAN_POINT('Ctrl Pts',(7.29140272492947,0.640759617553892,5.69737175715812));
#8804=CARTESIAN_POINT('Ctrl Pts',(7.32588776974505,0.246065794644022,5.96496491665055));
#8805=CARTESIAN_POINT('Ctrl Pts',(7.35362729609519,-0.118440598074296,5.97657459585275));
#8806=CARTESIAN_POINT('Ctrl Pts',(7.37682808694136,-0.405776263850554,5.87592416000432));
#8807=CARTESIAN_POINT('Ctrl Pts',(7.40246011243668,-0.649742181768781,5.63708400277588));
#8808=CARTESIAN_POINT('Ctrl Pts',(7.43055732482948,-0.759491260397883,5.27939247550575));
#8809=CARTESIAN_POINT('Ctrl Pts',(7.45408328696561,-0.696658442318083,4.97251220294606));
#8810=CARTESIAN_POINT('Ctrl Pts',(7.47297033777351,-0.562772704954616,4.76656163926831));
#8811=CARTESIAN_POINT('Ctrl Pts',(7.49190239095096,-0.381972617311867,4.59904546261976));
#8812=CARTESIAN_POINT('Ctrl Pts',(7.51565348005123,-0.0879986165622313,
4.48426496479248));
#8813=CARTESIAN_POINT('Ctrl Pts',(7.54905384695099,0.354151719711531,4.53895015859063));
#8814=CARTESIAN_POINT('Ctrl Pts',(7.58025012786886,0.669708281866875,4.83233675359967));
#8815=CARTESIAN_POINT('Ctrl Pts',(7.60918908886255,0.766049363842592,5.20056109169432));
#8816=CARTESIAN_POINT('Ctrl Pts',(7.63822532543653,0.724677250086816,5.57929734522926));
#8817=CARTESIAN_POINT('Ctrl Pts',(7.67470077570181,0.410318385521739,5.97456130664251));
#8818=CARTESIAN_POINT('Ctrl Pts',(7.71507638215079,-0.142205641163269,6.05698865126465));
#8819=CARTESIAN_POINT('Ctrl Pts',(7.75197857351751,-0.575616781704155,5.81621148710719));
#8820=CARTESIAN_POINT('Ctrl Pts',(7.7853417233448,-0.792188660547873,5.42454893449295));
#8821=CARTESIAN_POINT('Ctrl Pts',(7.81047387915203,-0.773098565169157,5.08768447811596));
#8822=CARTESIAN_POINT('Ctrl Pts',(7.82726838473859,-0.686808914769296,4.88823688066732));
#8823=CARTESIAN_POINT('Ctrl Pts',(7.835674306709,-0.630239891545833,4.7953931849875));
#8824=CARTESIAN_POINT('Ctrl Pts',(7.84408881413366,-0.561096499472987,4.71120959694044));
#8825=CARTESIAN_POINT('Ctrl Pts',(7.85719169921437,-0.436283161532637,4.59679757004653));
#8826=CARTESIAN_POINT('Ctrl Pts',(7.88250981486252,-0.142222857964216,4.43951581665192));
#8827=CARTESIAN_POINT('Ctrl Pts',(7.91639613701036,0.324197674501624,4.47456645604085));
#8828=CARTESIAN_POINT('Ctrl Pts',(7.95421610770856,0.703178520684008,4.8144802854019));
#8829=CARTESIAN_POINT('Ctrl Pts',(7.98837804458697,0.83019336282416,5.25430147573914));
#8830=CARTESIAN_POINT('Ctrl Pts',(8.02265345717082,0.703100029192506,5.69683666807885));
#8831=CARTESIAN_POINT('Ctrl Pts',(8.05703932219342,0.359082622660234,6.00447747470694));
#8832=CARTESIAN_POINT('Ctrl Pts',(8.09152885121967,-0.0973054214259819,
6.08243030040749));
#8833=CARTESIAN_POINT('Ctrl Pts',(8.12611659734114,-0.526430256741482,5.90506932981871));
#8834=CARTESIAN_POINT('Ctrl Pts',(8.16079619608074,-0.796185325416799,5.5256490871169));
#8835=CARTESIAN_POINT('Ctrl Pts',(8.19556142276615,-0.822839939891373,5.05970301502219));
#8836=CARTESIAN_POINT('Ctrl Pts',(8.2304057358346,-0.597042136063547,4.65004920673372));
#8837=CARTESIAN_POINT('Ctrl Pts',(8.26532250261526,-0.187078096730767,4.42280111950569));
#8838=CARTESIAN_POINT('Ctrl Pts',(8.30030493712832,0.281835625706235,4.44849940120078));
#8839=CARTESIAN_POINT('Ctrl Pts',(8.335346094925,0.665868121349874,4.72015532769358));
#8840=CARTESIAN_POINT('Ctrl Pts',(8.37043908067028,0.846830207518658,5.15510382746606));
#8841=CARTESIAN_POINT('Ctrl Pts',(8.40557652216204,0.76856474297763,5.62027880248826));
#8842=CARTESIAN_POINT('Ctrl Pts',(8.44075186874733,0.454573489708275,5.9728735479694));
#8843=CARTESIAN_POINT('Ctrl Pts',(8.47595655163873,0.000592216545345121,
6.10462424972125));
#8844=CARTESIAN_POINT('Ctrl Pts',(8.50531485448479,-0.378126834876055,5.99608292083659));
#8845=CARTESIAN_POINT('Ctrl Pts',(8.52880549491824,-0.61220217773172,5.79865133938525));
#8846=CARTESIAN_POINT('Ctrl Pts',(8.55099425377555,-0.773619699372566,5.55873173979293));
#8847=CARTESIAN_POINT('Ctrl Pts',(8.57776180819305,-0.845133662349741,5.20958202612232));
#8848=CARTESIAN_POINT('Ctrl Pts',(8.60909324987135,-0.722872864715742,4.81086604976394));
#8849=CARTESIAN_POINT('Ctrl Pts',(8.63781260447889,-0.449832178475452,4.54300286426828));
#8850=CARTESIAN_POINT('Ctrl Pts',(8.66391301341504,-0.126615872418881,4.42985501290241));
#8851=CARTESIAN_POINT('Ctrl Pts',(8.69522182105708,0.284827089964824,4.44259765149754));
#8852=CARTESIAN_POINT('Ctrl Pts',(8.73433751096835,0.733021979172566,4.74531837229694));
#8853=CARTESIAN_POINT('Ctrl Pts',(8.78121985601859,0.879026849711619,5.37848771966574));
#8854=CARTESIAN_POINT('Ctrl Pts',(8.82802879092876,0.556658256670406,5.94020744536304));
#8855=CARTESIAN_POINT('Ctrl Pts',(8.87474682574646,-0.0611139932480479,
6.13293868276154));
#8856=CARTESIAN_POINT('Ctrl Pts',(8.913590527633,-0.545669664063004,5.90050291517835));
#8857=CARTESIAN_POINT('Ctrl Pts',(8.94460190831635,-0.761866942586277,5.55563994385839));
#8858=CARTESIAN_POINT('Ctrl Pts',(8.97556820450398,-0.840825162899319,5.15613185120987));
#8859=CARTESIAN_POINT('Ctrl Pts',(9.00904197636457,-0.673477940739932,4.72513624475881));
#8860=CARTESIAN_POINT('Ctrl Pts',(9.04498768824832,-0.271018916657287,4.46467281490372));
#8861=CARTESIAN_POINT('Ctrl Pts',(9.07572502891324,0.136431921301358,4.4323095041422));
#8862=CARTESIAN_POINT('Ctrl Pts',(9.1076623520104,0.525083004968427,4.60584001971559));
#8863=CARTESIAN_POINT('Ctrl Pts',(9.14078441660845,0.783740757738325,4.96735319118576));
#8864=CARTESIAN_POINT('Ctrl Pts',(9.17506955917779,0.811435257145466,5.42693255065578));
#8865=CARTESIAN_POINT('Ctrl Pts',(9.20923929276318,0.591126060121817,5.82930504824957));
#8866=CARTESIAN_POINT('Ctrl Pts',(9.2432856375487,0.191952178313332,6.05209191391443));
#8867=CARTESIAN_POINT('Ctrl Pts',(9.27720741279787,-0.262891492169015,6.02844633536177));
#8868=CARTESIAN_POINT('Ctrl Pts',(9.31098858952086,-0.63403272803984,5.76750123179495));
#8869=CARTESIAN_POINT('Ctrl Pts',(9.34464578869081,-0.808786198417316,5.35074288886772));
#8870=CARTESIAN_POINT('Ctrl Pts',(9.37812199499848,-0.735387937206534,4.90681109950957));
#8871=CARTESIAN_POINT('Ctrl Pts',(9.41152322842209,-0.438313831815708,4.5712184418284));
#8872=CARTESIAN_POINT('Ctrl Pts',(9.43907484027071,-0.0815663109302454,
4.4669012937477));
#8873=CARTESIAN_POINT('Ctrl Pts',(9.4612729336839,0.203489644522288,4.50602296930772));
#8874=CARTESIAN_POINT('Ctrl Pts',(9.48288145933666,0.466474214399761,4.62164830317789));
#8875=CARTESIAN_POINT('Ctrl Pts',(9.50600861598851,0.663637471981693,4.83989009112341));
#8876=CARTESIAN_POINT('Ctrl Pts',(9.5237504983284,0.740394735416907,5.07762350734759));
#8877=CARTESIAN_POINT('Ctrl Pts',(9.53653973758647,0.755044636738244,5.21674586453469));
#8878=CARTESIAN_POINT('Ctrl Pts',(9.54057094671748,0.75177110427318,5.31144642435382));
#8879=CARTESIAN_POINT('Ctrl Pts',(9.54219323251979,0.741887195738976,5.37894319660566));
#8880=CARTESIAN_POINT('Ctrl Pts',(9.5445220671336,0.730934116011717,5.43050504199544));
#8881=CARTESIAN_POINT('Ctrl Pts',(9.54653892088636,0.71606192719596,5.48162749166749));
#8882=CARTESIAN_POINT('Ctrl Pts',(9.55030275855579,0.679655812307881,5.58080645949484));
#8883=CARTESIAN_POINT('Ctrl Pts',(9.55628190241597,0.599176010120261,5.71884228830231));
#8884=CARTESIAN_POINT('Ctrl Pts',(9.56403888456,0.445318424533598,5.86575289756921));
#8885=CARTESIAN_POINT('Ctrl Pts',(9.57187432376913,0.256949209836898,5.96422582543611));
#8886=CARTESIAN_POINT('Ctrl Pts',(9.57966347320304,0.0489975353055775,6.00644848836681));
#8887=CARTESIAN_POINT('Ctrl Pts',(9.59005920748721,-0.232880677765524,5.98418877373988));
#8888=CARTESIAN_POINT('Ctrl Pts',(9.60301490728257,-0.551448605271625,5.809856277591));
#8889=CARTESIAN_POINT('Ctrl Pts',(9.6185356227464,-0.762994742028112,5.42967706691061));
#8890=CARTESIAN_POINT('Ctrl Pts',(9.63401589798779,-0.739733408664225,4.99657949737655));
#8891=CARTESIAN_POINT('Ctrl Pts',(9.64945947119682,-0.490079410801249,4.64296802543169));
#8892=CARTESIAN_POINT('Ctrl Pts',(9.66486611496518,-0.0914480651653445,
4.47748174052505));
#8893=CARTESIAN_POINT('Ctrl Pts',(9.68023447346001,0.333029170036261,4.5489404444483));
#8894=CARTESIAN_POINT('Ctrl Pts',(9.69556462598151,0.653376293098328,4.83529182895193));
#8895=CARTESIAN_POINT('Ctrl Pts',(9.70575657704672,0.732335431233298,5.10911134118588));
#8896=CARTESIAN_POINT('Ctrl Pts',(9.71084842832256,0.732353944732881,5.24663464006324));
#8897=CARTESIAN_POINT('Ctrl Pts',(6.53677890889994,0.648308344097312,5.24788808861526));
#8898=CARTESIAN_POINT('Ctrl Pts',(6.54128841999409,0.648291947932169,5.36968324994926));
#8899=CARTESIAN_POINT('Ctrl Pts',(6.55029072386857,0.578366883190402,5.61148400116062));
#8900=CARTESIAN_POINT('Ctrl Pts',(6.56377552959342,0.296488302798292,5.86313472695387));
#8901=CARTESIAN_POINT('Ctrl Pts',(6.57723486151276,-0.0753487981176404,
5.92558903258212));
#8902=CARTESIAN_POINT('Ctrl Pts',(6.59067201260385,-0.422743869195993,5.78083317969924));
#8903=CARTESIAN_POINT('Ctrl Pts',(6.60408642445702,-0.639583194854741,5.47384153684459));
#8904=CARTESIAN_POINT('Ctrl Pts',(6.61747718701865,-0.659388633790789,5.09914333460697));
#8905=CARTESIAN_POINT('Ctrl Pts',(6.63084921534714,-0.477002675415156,4.77178831487133));
#8906=CARTESIAN_POINT('Ctrl Pts',(6.64196797156513,-0.203535776818503,4.62233154714453));
#8907=CARTESIAN_POINT('Ctrl Pts',(6.65086270156841,0.0376212461558179,4.60332808393359));
#8908=CARTESIAN_POINT('Ctrl Pts',(6.65751436882366,0.215206656454501,4.63940682661395));
#8909=CARTESIAN_POINT('Ctrl Pts',(6.66419350349961,0.375739235616664,4.72336011101286));
#8910=CARTESIAN_POINT('Ctrl Pts',(6.67079173242759,0.506648525281715,4.84836014585996));
#8911=CARTESIAN_POINT('Ctrl Pts',(6.67587168733797,0.574942135378562,4.96558591415989));
#8912=CARTESIAN_POINT('Ctrl Pts',(6.67905830408769,0.605836587356559,5.0496479041938));
#8913=CARTESIAN_POINT('Ctrl Pts',(6.68075445132886,0.61822311366418,5.09247873674454));
#8914=CARTESIAN_POINT('Ctrl Pts',(6.68271633522742,0.627705254751127,5.13628244164802));
#8915=CARTESIAN_POINT('Ctrl Pts',(6.68424751516306,0.636157930364232,5.19641973994768));
#8916=CARTESIAN_POINT('Ctrl Pts',(6.68721504263871,0.638850758901545,5.26817630302783));
#8917=CARTESIAN_POINT('Ctrl Pts',(6.6980886411611,0.626432492962911,5.38747198490893));
#8918=CARTESIAN_POINT('Ctrl Pts',(6.7130742817883,0.561598102708803,5.58757297033252));
#8919=CARTESIAN_POINT('Ctrl Pts',(6.73247121050942,0.395939555636536,5.77092466279022));
#8920=CARTESIAN_POINT('Ctrl Pts',(6.75050076668837,0.176511931668019,5.86718938307879));
#8921=CARTESIAN_POINT('Ctrl Pts',(6.76896343885092,-0.0605850594853099,
5.89971030240676));
#8922=CARTESIAN_POINT('Ctrl Pts',(6.79176314959733,-0.35582242285045,5.81305067264655));
#8923=CARTESIAN_POINT('Ctrl Pts',(6.81822260673932,-0.590783555636119,5.54697381679167));
#8924=CARTESIAN_POINT('Ctrl Pts',(6.84357792410812,-0.655910626230322,5.21520740643816));
#8925=CARTESIAN_POINT('Ctrl Pts',(6.86792311414774,-0.558797745057059,4.90596294050986));
#8926=CARTESIAN_POINT('Ctrl Pts',(6.89223845562662,-0.325774686137532,4.68084210219441));
#8927=CARTESIAN_POINT('Ctrl Pts',(6.91655009079728,-0.0137382982285809,
4.59469205345031));
#8928=CARTESIAN_POINT('Ctrl Pts',(6.94085000037151,0.301406716506307,4.66808590961898));
#8929=CARTESIAN_POINT('Ctrl Pts',(6.96312145304551,0.522894871174355,4.86564283981171));
#8930=CARTESIAN_POINT('Ctrl Pts',(6.98336932148207,0.627613721193077,5.10972341863593));
#8931=CARTESIAN_POINT('Ctrl Pts',(7.00767034974037,0.639345410745925,5.42926415376025));
#8932=CARTESIAN_POINT('Ctrl Pts',(7.0340061377139,0.456096194913984,5.74332463138044));
#8933=CARTESIAN_POINT('Ctrl Pts',(7.06239212271459,0.110146516358368,5.89696458325904));
#8934=CARTESIAN_POINT('Ctrl Pts',(7.08674403780546,-0.212777772472184,5.87153444736802));
#8935=CARTESIAN_POINT('Ctrl Pts',(7.10604298073846,-0.428203986860686,5.73123639550283));
#8936=CARTESIAN_POINT('Ctrl Pts',(7.1202763794347,-0.539896968044911,5.58432836902718));
#8937=CARTESIAN_POINT('Ctrl Pts',(7.13248259304633,-0.610589669953036,5.44288429135274));
#8938=CARTESIAN_POINT('Ctrl Pts',(7.15386080729459,-0.662907145870833,5.16664121175135));
#8939=CARTESIAN_POINT('Ctrl Pts',(7.18445524346917,-0.507518708932404,4.77315870520267));
#8940=CARTESIAN_POINT('Ctrl Pts',(7.2212730060695,-0.0473329540045874,4.55302086919988));
#8941=CARTESIAN_POINT('Ctrl Pts',(7.25821128490183,0.440889209665914,4.70515440715441));
#8942=CARTESIAN_POINT('Ctrl Pts',(7.29528590651588,0.696637153045051,5.15010859139779));
#8943=CARTESIAN_POINT('Ctrl Pts',(7.332512739643,0.58082551013422,5.65279628754744));
#8944=CARTESIAN_POINT('Ctrl Pts',(7.3636735148449,0.224022453087409,5.89445423698418));
#8945=CARTESIAN_POINT('Ctrl Pts',(7.38869394277869,-0.104770142311705,5.9048883954555));
#8946=CARTESIAN_POINT('Ctrl Pts',(7.4095969054791,-0.363665133915886,5.81417857686521));
#8947=CARTESIAN_POINT('Ctrl Pts',(7.43265719036872,-0.583169551820776,5.59922290709689));
#8948=CARTESIAN_POINT('Ctrl Pts',(7.45790499477554,-0.681772872980722,5.27773207396749));
#8949=CARTESIAN_POINT('Ctrl Pts',(7.47902438387107,-0.625327749884945,5.00220880580607));
#8950=CARTESIAN_POINT('Ctrl Pts',(7.49596985369807,-0.505194085748851,4.81741578549234));
#8951=CARTESIAN_POINT('Ctrl Pts',(7.51294825933135,-0.343029342279038,4.66716861489283));
#8952=CARTESIAN_POINT('Ctrl Pts',(7.53423229204698,-0.0795149396536471,
4.56430162846121));
#8953=CARTESIAN_POINT('Ctrl Pts',(7.56415795707461,0.316651231938915,4.61331432755186));
#8954=CARTESIAN_POINT('Ctrl Pts',(7.59208894080855,0.599222510850577,4.8760718061598));
#8955=CARTESIAN_POINT('Ctrl Pts',(7.61800089328846,0.685499071631382,5.20580221532286));
#8956=CARTESIAN_POINT('Ctrl Pts',(7.64399762025679,0.648452480668231,5.5449492628021));
#8957=CARTESIAN_POINT('Ctrl Pts',(7.6766558308975,0.366948218153944,5.89895940428666));
#8958=CARTESIAN_POINT('Ctrl Pts',(7.71283041368628,-0.128170599844781,5.97289577401557));
#8959=CARTESIAN_POINT('Ctrl Pts',(7.74591955350209,-0.516915920064396,5.75700818829182));
#8960=CARTESIAN_POINT('Ctrl Pts',(7.77585687382348,-0.711357071237054,5.4054746092851));
#8961=CARTESIAN_POINT('Ctrl Pts',(7.79843023324687,-0.694254716447698,5.10278765610887));
#8962=CARTESIAN_POINT('Ctrl Pts',(7.81353402254503,-0.616644573867706,4.92340025453556));
#8963=CARTESIAN_POINT('Ctrl Pts',(7.82109624603377,-0.565750095788821,4.83986786624699));
#8964=CARTESIAN_POINT('Ctrl Pts',(7.82866883860509,-0.503521173252006,4.76409997528913));
#8965=CARTESIAN_POINT('Ctrl Pts',(7.84046426369671,-0.391150332502584,4.66109170486198));
#8966=CARTESIAN_POINT('Ctrl Pts',(7.86326838969153,-0.126269457842156,4.51937164453054));
#8967=CARTESIAN_POINT('Ctrl Pts',(7.89384459534472,0.294624621968566,4.55083813829548));
#8968=CARTESIAN_POINT('Ctrl Pts',(7.92803343879433,0.637390764050739,4.85808320500068));
#8969=CARTESIAN_POINT('Ctrl Pts',(7.95897115106736,0.752557991506694,5.25650008748354));
#8970=CARTESIAN_POINT('Ctrl Pts',(7.99008150777189,0.637292674479974,5.6583098830911));
#8971=CARTESIAN_POINT('Ctrl Pts',(8.02136268813123,0.324328340887489,5.93835687143453));
#8972=CARTESIAN_POINT('Ctrl Pts',(8.05281552085117,-0.0919668369256177,
6.0096089960033));
#8973=CARTESIAN_POINT('Ctrl Pts',(8.08443922850855,-0.484488081008684,5.84754699761468));
#8974=CARTESIAN_POINT('Ctrl Pts',(8.11623331579657,-0.732001743146474,5.49969950716172));
#8975=CARTESIAN_POINT('Ctrl Pts',(8.14819672239933,-0.756691626879712,5.07120150721029));
#8976=CARTESIAN_POINT('Ctrl Pts',(8.18032818682298,-0.548581427785167,4.69325383595664));
#8977=CARTESIAN_POINT('Ctrl Pts',(8.21262609933926,-0.169361160919892,4.48282710725417));
#8978=CARTESIAN_POINT('Ctrl Pts',(8.24508852965908,0.265897639458044,4.50648066670812));
#8979=CARTESIAN_POINT('Ctrl Pts',(8.27771329285446,0.623659903118161,4.7592998152198));
#8980=CARTESIAN_POINT('Ctrl Pts',(8.31049776406179,0.792961734420276,5.16566132423459));
#8981=CARTESIAN_POINT('Ctrl Pts',(8.34343929891669,0.719787629314293,5.60191531751229));
#8982=CARTESIAN_POINT('Ctrl Pts',(8.3765342962972,0.424457038652123,5.9339034705343));
#8983=CARTESIAN_POINT('Ctrl Pts',(8.40978030794087,-0.00430578935872142,
6.05858175740242));
#8984=CARTESIAN_POINT('Ctrl Pts',(8.43760606022993,-0.363432150149208,5.9558615895779));
#8985=CARTESIAN_POINT('Ctrl Pts',(8.45994080550056,-0.58605591073669,5.76814595608163));
#8986=CARTESIAN_POINT('Ctrl Pts',(8.48107939877234,-0.73987545479849,5.53958299989996));
#8987=CARTESIAN_POINT('Ctrl Pts',(8.5066384857038,-0.808346850487237,5.20610228318772));
#8988=CARTESIAN_POINT('Ctrl Pts',(8.53667295472767,-0.691293438814756,4.82379987835255));
#8989=CARTESIAN_POINT('Ctrl Pts',(8.56429709374726,-0.42873318070134,4.56597536887464));
#8990=CARTESIAN_POINT('Ctrl Pts',(8.58948347459684,-0.116793468377635,4.45670239484369));
#8991=CARTESIAN_POINT('Ctrl Pts',(8.61978105797819,0.281366713802581,4.46891907801678));
#8992=CARTESIAN_POINT('Ctrl Pts',(8.65778272897614,0.717169109368427,4.76263678021251));
#8993=CARTESIAN_POINT('Ctrl Pts',(8.70358396899606,0.86049511964979,5.38117382901366));
#8994=CARTESIAN_POINT('Ctrl Pts',(8.74957058756189,0.544301662499638,5.93347229333488));
#8995=CARTESIAN_POINT('Ctrl Pts',(8.79572865872733,-0.0659692059206899,
6.12458004624303));
#8996=CARTESIAN_POINT('Ctrl Pts',(8.83432310014984,-0.547772509862173,5.89408580556368));
#8997=CARTESIAN_POINT('Ctrl Pts',(8.86527036286416,-0.763656389723532,5.54991022181832));
#8998=CARTESIAN_POINT('Ctrl Pts',(8.89626292036845,-0.842796411694417,5.15009597609929));
#8999=CARTESIAN_POINT('Ctrl Pts',(8.92990401221682,-0.675022169192827,4.71671716418602));
#9000=CARTESIAN_POINT('Ctrl Pts',(8.9662054975265,-0.26866399657737,4.4534420925465));
#9001=CARTESIAN_POINT('Ctrl Pts',(8.99736409597451,0.144379983188026,4.4204521703534));
#9002=CARTESIAN_POINT('Ctrl Pts',(9.02986103725035,0.539947482583334,4.59684672007972));
#9003=CARTESIAN_POINT('Ctrl Pts',(9.06369328425281,0.804398444941881,4.96601673371496));
#9004=CARTESIAN_POINT('Ctrl Pts',(9.09886203052067,0.833075652533933,5.43747935159163));
#9005=CARTESIAN_POINT('Ctrl Pts',(9.13405836073647,0.606349827859166,5.8521164848996));
#9006=CARTESIAN_POINT('Ctrl Pts',(9.16927256307506,0.193565787562334,6.08279802034468));
#9007=CARTESIAN_POINT('Ctrl Pts',(9.20450120399963,-0.278862713204365,6.05849885410467));
#9008=CARTESIAN_POINT('Ctrl Pts',(9.23972501673659,-0.666042337314815,5.78659268801242));
#9009=CARTESIAN_POINT('Ctrl Pts',(9.27495928577355,-0.849238451522511,5.35036898675046));
#9010=CARTESIAN_POINT('Ctrl Pts',(9.3101402023598,-0.77235128088339,4.88373310289506));
#9011=CARTESIAN_POINT('Ctrl Pts',(9.34537826519511,-0.459114700993423,4.52949905625442));
#9012=CARTESIAN_POINT('Ctrl Pts',(9.37455217501767,-0.0813826670684427,
4.41879392741861));
#9013=CARTESIAN_POINT('Ctrl Pts',(9.39812483474283,0.221347040696434,4.46032370541366));
#9014=CARTESIAN_POINT('Ctrl Pts',(9.42111143712525,0.501106191970378,4.58320002284348));
#9015=CARTESIAN_POINT('Ctrl Pts',(9.44577928522819,0.711600998294542,4.81615110634447));
#9016=CARTESIAN_POINT('Ctrl Pts',(9.46476901472948,0.793754078120072,5.07020874147712));
#9017=CARTESIAN_POINT('Ctrl Pts',(9.4784973521178,0.809459762090862,5.22012003835188));
#9018=CARTESIAN_POINT('Ctrl Pts',(9.48256220237874,0.80599714391194,5.31678427772113));
#9019=CARTESIAN_POINT('Ctrl Pts',(9.48439284136576,0.79535027000064,5.39088618359879));
#9020=CARTESIAN_POINT('Ctrl Pts',(9.4868839869042,0.783486446136706,5.44625321444756));
#9021=CARTESIAN_POINT('Ctrl Pts',(9.48903979693529,0.76765908397162,5.50080528896331));
#9022=CARTESIAN_POINT('Ctrl Pts',(9.49307526895426,0.728584239469491,5.60719555343428));
#9023=CARTESIAN_POINT('Ctrl Pts',(9.49949589017351,0.642208233985685,5.75539627308332));
#9024=CARTESIAN_POINT('Ctrl Pts',(9.50782995020485,0.476882658707867,5.91325735933798));
#9025=CARTESIAN_POINT('Ctrl Pts',(9.51625602332589,0.274333603849002,6.0191596722041));
#9026=CARTESIAN_POINT('Ctrl Pts',(9.52463871614711,0.0505347313054355,6.06461215503176));
#9027=CARTESIAN_POINT('Ctrl Pts',(9.53583562734331,-0.253057457619835,6.04065652197636));
#9028=CARTESIAN_POINT('Ctrl Pts',(9.5498071049154,-0.596622179197612,5.85274547177686));
#9029=CARTESIAN_POINT('Ctrl Pts',(9.56657059349091,-0.825178633194954,5.44220828219499));
#9030=CARTESIAN_POINT('Ctrl Pts',(9.58331580941746,-0.800115741031158,4.97374519727449));
#9031=CARTESIAN_POINT('Ctrl Pts',(9.60004749969833,-0.529743331948014,4.59064885817877));
#9032=CARTESIAN_POINT('Ctrl Pts',(9.61676192682012,-0.0973151100553377,
4.41101912125671));
#9033=CARTESIAN_POINT('Ctrl Pts',(9.63346072597428,0.363869421061874,4.48860536541958));
#9034=CARTESIAN_POINT('Ctrl Pts',(9.65013784702028,0.712465653120617,4.80001782474214));
#9035=CARTESIAN_POINT('Ctrl Pts',(9.66124801098291,0.79856285759502,5.09847089746305));
#9036=CARTESIAN_POINT('Ctrl Pts',(9.66679389193444,0.798583021904447,5.24825685984085));
#9037=CARTESIAN_POINT('Ctrl Pts',(6.55985766373767,0.695773542681336,5.24703997894806));
#9038=CARTESIAN_POINT('Ctrl Pts',(6.56469408527635,0.695755957900061,5.37766450326637));
#9039=CARTESIAN_POINT('Ctrl Pts',(6.57435500114752,0.620735066792372,5.6371846277021));
#9040=CARTESIAN_POINT('Ctrl Pts',(6.58881199472521,0.318467016967517,5.90695568638057));
#9041=CARTESIAN_POINT('Ctrl Pts',(6.60323442988062,-0.0799854836502877,
5.97386387712081));
#9042=CARTESIAN_POINT('Ctrl Pts',(6.61762277610453,-0.451981525128358,5.81879973852038));
#9043=CARTESIAN_POINT('Ctrl Pts',(6.63197659243013,-0.68398248083499,5.49026587240634));
#9044=CARTESIAN_POINT('Ctrl Pts',(6.64629279495561,-0.705102229235322,5.08960601326795));
#9045=CARTESIAN_POINT('Ctrl Pts',(6.66057898517367,-0.510181991891156,4.73986607438693));
#9046=CARTESIAN_POINT('Ctrl Pts',(6.6724472572393,-0.218209859199235,4.58035203049584));
#9047=CARTESIAN_POINT('Ctrl Pts',(6.68193687531017,0.039087393851036,4.56008746412766));
#9048=CARTESIAN_POINT('Ctrl Pts',(6.68903012532506,0.228476658021195,4.59857220869176));
#9049=CARTESIAN_POINT('Ctrl Pts',(6.6961496976064,0.399596133977577,4.68807212672819));
#9050=CARTESIAN_POINT('Ctrl Pts',(6.7031795050705,0.539084893132951,4.8212679598734));
#9051=CARTESIAN_POINT('Ctrl Pts',(6.70858995882373,0.611801754599193,4.94611855978549));
#9052=CARTESIAN_POINT('Ctrl Pts',(6.71198117635767,0.644700212006901,5.03560603181988));
#9053=CARTESIAN_POINT('Ctrl Pts',(6.71378304218766,0.657824365352093,5.08106104415238));
#9054=CARTESIAN_POINT('Ctrl Pts',(6.71586810234351,0.667974015272807,5.12771890448726));
#9055=CARTESIAN_POINT('Ctrl Pts',(6.71754218374966,0.676993827699967,5.19256731455862));
#9056=CARTESIAN_POINT('Ctrl Pts',(6.72057460952299,0.679835899888414,5.26655099041801));
#9057=CARTESIAN_POINT('Ctrl Pts',(6.73215258919641,0.666622431758416,5.39385244351734));
#9058=CARTESIAN_POINT('Ctrl Pts',(6.74808267646998,0.597703234226131,5.60637135858773));
#9059=CARTESIAN_POINT('Ctrl Pts',(6.76865865045639,0.42187569508026,5.80093567049644));
#9060=CARTESIAN_POINT('Ctrl Pts',(6.78775275289436,0.18949258292913,5.90281901720052));
#9061=CARTESIAN_POINT('Ctrl Pts',(6.80728398696971,-0.0613342485858974,
5.93720923449836));
#9062=CARTESIAN_POINT('Ctrl Pts',(6.83135970851047,-0.373059821574549,5.84556085535134));
#9063=CARTESIAN_POINT('Ctrl Pts',(6.85923191629717,-0.620447637519185,5.56518912958432));
#9064=CARTESIAN_POINT('Ctrl Pts',(6.88587504766456,-0.688763467578774,5.216551997357));
#9065=CARTESIAN_POINT('Ctrl Pts',(6.91139566465253,-0.586858521375168,4.89242219675425));
#9066=CARTESIAN_POINT('Ctrl Pts',(6.93682192897835,-0.343119258487298,4.6571125514519));
#9067=CARTESIAN_POINT('Ctrl Pts',(6.96217719555826,-0.017670596412725,4.56737841010226));
#9068=CARTESIAN_POINT('Ctrl Pts',(6.98745330968432,0.310091855530511,4.64383222378311));
#9069=CARTESIAN_POINT('Ctrl Pts',(7.01055807494553,0.539755215825518,4.8488411700511));
#9070=CARTESIAN_POINT('Ctrl Pts',(7.03150987721236,0.648059883045342,5.10140557124907));
#9071=CARTESIAN_POINT('Ctrl Pts',(7.05660277782412,0.660088135117788,5.43135081654961));
#9072=CARTESIAN_POINT('Ctrl Pts',(7.08371253109927,0.471238232523407,5.75442284803613));
#9073=CARTESIAN_POINT('Ctrl Pts',(7.11281790701897,0.116492402038094,5.91178575585197));
#9074=CARTESIAN_POINT('Ctrl Pts',(7.13771330081894,-0.213583901535594,5.88567475580613));
#9075=CARTESIAN_POINT('Ctrl Pts',(7.15738807567549,-0.433075159347389,5.74259656511571));
#9076=CARTESIAN_POINT('Ctrl Pts',(7.17186233961118,-0.546637546600257,5.59321236996226));
#9077=CARTESIAN_POINT('Ctrl Pts',(7.18426142057677,-0.618429896637663,5.44955013009039));
#9078=CARTESIAN_POINT('Ctrl Pts',(7.20593925357481,-0.671404712921254,5.16944154295922));
#9079=CARTESIAN_POINT('Ctrl Pts',(7.23685805149232,-0.514056507473933,4.7720238817847));
#9080=CARTESIAN_POINT('Ctrl Pts',(7.27388829057188,-0.0511187931748622,
4.55109735415634));
#9081=CARTESIAN_POINT('Ctrl Pts',(7.31086361178906,0.437321455158784,4.70378519211358));
#9082=CARTESIAN_POINT('Ctrl Pts',(7.34779990172598,0.691641488782215,5.14718657589742));
#9083=CARTESIAN_POINT('Ctrl Pts',(7.38471185454084,0.576388219284925,5.64538232477128));
#9084=CARTESIAN_POINT('Ctrl Pts',(7.41546811917344,0.224145749390111,5.88350929405959));
#9085=CARTESIAN_POINT('Ctrl Pts',(7.44007339032313,-0.0991038282370662,
5.89369455116736));
#9086=CARTESIAN_POINT('Ctrl Pts',(7.46058115581319,-0.353046546940354,5.80465440934753));
#9087=CARTESIAN_POINT('Ctrl Pts',(7.48315729994566,-0.567747214692048,5.59423252752844));
#9088=CARTESIAN_POINT('Ctrl Pts',(7.50779960123253,-0.663810701459249,5.28055053342104));
#9089=CARTESIAN_POINT('Ctrl Pts',(7.52834941587818,-0.608816343721552,5.01257565766459));
#9090=CARTESIAN_POINT('Ctrl Pts',(7.54479896304165,-0.492201788139917,4.83323933395727));
#9091=CARTESIAN_POINT('Ctrl Pts',(7.56125874789373,-0.335011840659567,4.68763787379617));
#9092=CARTESIAN_POINT('Ctrl Pts',(7.58185937612452,-0.0800643356826357,
4.58819992347848));
#9093=CARTESIAN_POINT('Ctrl Pts',(7.61072436677918,0.302026124742895,4.63563761482126));
#9094=CARTESIAN_POINT('Ctrl Pts',(7.63759060214969,0.573543629548249,4.88843827187382));
#9095=CARTESIAN_POINT('Ctrl Pts',(7.66243418548257,0.656176634414132,5.20452875813442));
#9096=CARTESIAN_POINT('Ctrl Pts',(7.68731798929925,0.620672834689613,5.52907101102389));
#9097=CARTESIAN_POINT('Ctrl Pts',(7.7185008361451,0.351786215425856,5.86676654532321));
#9098=CARTESIAN_POINT('Ctrl Pts',(7.75291850276096,-0.119163757158855,5.93680388820774));
#9099=CARTESIAN_POINT('Ctrl Pts',(7.78431371344778,-0.487788664582144,5.73191159498108));
#9100=CARTESIAN_POINT('Ctrl Pts',(7.81266278264196,-0.671728137594293,5.39915542463631));
#9101=CARTESIAN_POINT('Ctrl Pts',(7.83399695974143,-0.655495509577423,5.11326864305501));
#9102=CARTESIAN_POINT('Ctrl Pts',(7.84824319365684,-0.582304862321808,4.94409375866328));
#9103=CARTESIAN_POINT('Ctrl Pts',(7.85537248762996,-0.534328882072017,4.8653541422696));
#9104=CARTESIAN_POINT('Ctrl Pts',(7.8625080462426,-0.475697660357833,4.79396953698449));
#9105=CARTESIAN_POINT('Ctrl Pts',(7.87361834107539,-0.369870381089617,4.69696159670125));
#9106=CARTESIAN_POINT('Ctrl Pts',(7.89508364408438,-0.120581127165717,4.56363681242408));
#9107=CARTESIAN_POINT('Ctrl Pts',(7.92380487431976,0.274740702833653,4.59333951805747));
#9108=CARTESIAN_POINT('Ctrl Pts',(7.95587209874155,0.596060666569318,4.88149726068058));
#9109=CARTESIAN_POINT('Ctrl Pts',(7.98485490982878,0.703850404186812,5.25458043203598));
#9110=CARTESIAN_POINT('Ctrl Pts',(8.01395674562579,0.596009128666447,5.63029687158413));
#9111=CARTESIAN_POINT('Ctrl Pts',(8.04318557856648,0.303669437197963,5.89183096604927));
#9112=CARTESIAN_POINT('Ctrl Pts',(8.07254379370764,-0.0847679250430139,
5.95827083698362));
#9113=CARTESIAN_POINT('Ctrl Pts',(8.10203585350491,-0.450682443971355,5.80715198412111));
#9114=CARTESIAN_POINT('Ctrl Pts',(8.13166487881109,-0.68123591985956,5.48308204769604));
#9115=CARTESIAN_POINT('Ctrl Pts',(8.16143417804738,-0.704196784100177,5.08412597468992));
#9116=CARTESIAN_POINT('Ctrl Pts',(8.19134657907665,-0.510502727194234,4.73239774783289));
#9117=CARTESIAN_POINT('Ctrl Pts',(8.22140471118437,-0.157680363027014,4.53663054946559));
#9118=CARTESIAN_POINT('Ctrl Pts',(8.25161091715579,0.247209806959665,4.55863531050862));
#9119=CARTESIAN_POINT('Ctrl Pts',(8.28196721226589,0.580007046161269,4.79380459237181));
#9120=CARTESIAN_POINT('Ctrl Pts',(8.31247546153882,0.737522986966818,5.17184248687906));
#9121=CARTESIAN_POINT('Ctrl Pts',(8.3431369636528,0.669452578237767,5.57779897785294));
#9122=CARTESIAN_POINT('Ctrl Pts',(8.37395338723204,0.394549325777573,5.88686270419447));
#9123=CARTESIAN_POINT('Ctrl Pts',(8.40492468218856,-0.00477288997479829,
6.00301968920375));
#9124=CARTESIAN_POINT('Ctrl Pts',(8.43086566271663,-0.339484126663846,5.90732172989766));
#9125=CARTESIAN_POINT('Ctrl Pts',(8.45169393946564,-0.547072218093633,5.73229404684569));
#9126=CARTESIAN_POINT('Ctrl Pts',(8.47141407618564,-0.69056376988887,5.51909409327636));
#9127=CARTESIAN_POINT('Ctrl Pts',(8.49528051079703,-0.754506655121167,5.20780227421841));
#9128=CARTESIAN_POINT('Ctrl Pts',(8.52334094921819,-0.645203605665545,4.85064301321389));
#9129=CARTESIAN_POINT('Ctrl Pts',(8.54917704999056,-0.39970756208167,4.60951445591631));
#9130=CARTESIAN_POINT('Ctrl Pts',(8.57275318463256,-0.107751104615898,4.507212319962));
#9131=CARTESIAN_POINT('Ctrl Pts',(8.60113510608758,0.2652008828398,4.51862276966196));
#9132=CARTESIAN_POINT('Ctrl Pts',(8.63678462905851,0.674063216653352,4.79397580501787));
#9133=CARTESIAN_POINT('Ctrl Pts',(8.67983312698351,0.808996095068133,5.37521245548929));
#9134=CARTESIAN_POINT('Ctrl Pts',(8.72314631206897,0.511438980015273,5.89547267476356));
#9135=CARTESIAN_POINT('Ctrl Pts',(8.76671889614431,-0.0645101499886897,
6.07612806192154));
#9136=CARTESIAN_POINT('Ctrl Pts',(8.8032403134946,-0.52050637307905,5.85824970323195));
#9137=CARTESIAN_POINT('Ctrl Pts',(8.8325806026404,-0.725222219240906,5.53197478069197));
#9138=CARTESIAN_POINT('Ctrl Pts',(8.86200208878909,-0.800401500077765,5.15246739538599));
#9139=CARTESIAN_POINT('Ctrl Pts',(8.89400332481794,-0.641019042589212,4.74014811866369));
#9140=CARTESIAN_POINT('Ctrl Pts',(8.92861674579342,-0.253623824855234,4.48900662534079));
#9141=CARTESIAN_POINT('Ctrl Pts',(8.95838394375014,0.14096968639971,4.45739530277337));
#9142=CARTESIAN_POINT('Ctrl Pts',(8.98949233523325,0.519678120112436,4.62614772615488));
#9143=CARTESIAN_POINT('Ctrl Pts',(9.02194827654078,0.773504466413702,4.98022549611561));
#9144=CARTESIAN_POINT('Ctrl Pts',(9.05576659670161,0.801241182054453,5.43359139583031));
#9145=CARTESIAN_POINT('Ctrl Pts',(9.08969328319026,0.582823669257135,5.83337236814146));
#9146=CARTESIAN_POINT('Ctrl Pts',(9.12372119491323,0.183995572608789,6.0564428736434));
#9147=CARTESIAN_POINT('Ctrl Pts',(9.15784898234373,-0.273721773698358,6.03306963582005));
#9148=CARTESIAN_POINT('Ctrl Pts',(9.19205946304498,-0.64990994575872,5.76909502946593));
#9149=CARTESIAN_POINT('Ctrl Pts',(9.22636972842826,-0.828492853046594,5.34432711727714));
#9150=CARTESIAN_POINT('Ctrl Pts',(9.26071770907781,-0.753605783690083,4.88862365787852));
#9151=CARTESIAN_POINT('Ctrl Pts',(9.29521525363159,-0.447059278266013,4.54166254803362));
#9152=CARTESIAN_POINT('Ctrl Pts',(9.32385029237493,-0.076279701533059,4.43278968651557));
#9153=CARTESIAN_POINT('Ctrl Pts',(9.34704014326617,0.221568143128904,4.47363161156646));
#9154=CARTESIAN_POINT('Ctrl Pts',(9.36968427093344,0.497170404037412,4.59457970634328));
#9155=CARTESIAN_POINT('Ctrl Pts',(9.39402695598823,0.705082520374241,4.82463961699335));
#9156=CARTESIAN_POINT('Ctrl Pts',(9.41282588021654,0.786411815723876,5.07581826482597));
#9157=CARTESIAN_POINT('Ctrl Pts',(9.42644889255394,0.801979646461018,5.22505406419157));
#9158=CARTESIAN_POINT('Ctrl Pts',(9.43026740530825,0.798586255767136,5.31688402203871));
#9159=CARTESIAN_POINT('Ctrl Pts',(9.43215588553443,0.787994469037129,5.3917373403362));
#9160=CARTESIAN_POINT('Ctrl Pts',(9.43462005636334,0.77613860227658,5.44667996217276));
#9161=CARTESIAN_POINT('Ctrl Pts',(9.43675115866262,0.76054929407017,5.50053294126675));
#9162=CARTESIAN_POINT('Ctrl Pts',(9.44075039513402,0.721790412703208,5.60601810317749));
#9163=CARTESIAN_POINT('Ctrl Pts',(9.44711962463945,0.636128021011656,5.75304946126482));
#9164=CARTESIAN_POINT('Ctrl Pts',(9.45539179372209,0.471989769111388,5.90978296204479));
#9165=CARTESIAN_POINT('Ctrl Pts',(9.46376143836203,0.270776729544522,6.01500122015827));
#9166=CARTESIAN_POINT('Ctrl Pts',(9.47209357577949,0.048287231388412,6.06019930129363));
#9167=CARTESIAN_POINT('Ctrl Pts',(9.48323123102129,-0.253737210486127,6.03638375835141));
#9168=CARTESIAN_POINT('Ctrl Pts',(9.49713889491815,-0.595891436056078,5.84933347763517));
#9169=CARTESIAN_POINT('Ctrl Pts',(9.51385076478022,-0.823899220520506,5.4399993249345));
#9170=CARTESIAN_POINT('Ctrl Pts',(9.53056720336839,-0.798968852716643,4.97220899366434));
#9171=CARTESIAN_POINT('Ctrl Pts',(9.54729162985791,-0.528727439187925,4.58909409304663));
#9172=CARTESIAN_POINT('Ctrl Pts',(9.56402480986213,-0.0957723892084128,
4.40913981479913));
#9173=CARTESIAN_POINT('Ctrl Pts',(9.58076647982355,0.366654087604734,4.48684308047902));
#9174=CARTESIAN_POINT('Ctrl Pts',(9.59750846260415,0.71671035870106,4.79943942469371));
#9175=CARTESIAN_POINT('Ctrl Pts',(9.60867719102009,0.803285765633916,5.09951966622228));
#9176=CARTESIAN_POINT('Ctrl Pts',(9.61425624009638,0.803306050539573,5.25020145011708));
#9177=CARTESIAN_POINT('Ctrl Pts',(6.55994469204049,0.719709328495781,5.24703997894806));
#9178=CARTESIAN_POINT('Ctrl Pts',(6.56494552765653,0.719691145920131,5.38210508200347));
#9179=CARTESIAN_POINT('Ctrl Pts',(6.57494016333875,0.642089168505731,5.65058609468785));
#9180=CARTESIAN_POINT('Ctrl Pts',(6.58989438616266,0.32941528595114,5.9296313569664));
#9181=CARTESIAN_POINT('Ctrl Pts',(6.60481477071411,-0.0827797453005289,
5.99886361370576));
#9182=CARTESIAN_POINT('Ctrl Pts',(6.61969980345594,-0.467619845512657,5.83844773036597));
#9183=CARTESIAN_POINT('Ctrl Pts',(6.63454965842308,-0.707639327219362,5.49857002500469));
#9184=CARTESIAN_POINT('Ctrl Pts',(6.64936061260475,-0.729495436544756,5.0840660001111));
#9185=CARTESIAN_POINT('Ctrl Pts',(6.66414030226907,-0.527844751315962,4.72224444577032));
#9186=CARTESIAN_POINT('Ctrl Pts',(6.67641810037933,-0.225796647591973,4.55722222010489));
#9187=CARTESIAN_POINT('Ctrl Pts',(6.68623494447203,0.0403746271135037,4.5362580751361));
#9188=CARTESIAN_POINT('Ctrl Pts',(6.69357256905876,0.236291461979514,4.57606849800983));
#9189=CARTESIAN_POINT('Ctrl Pts',(6.70093718034598,0.413303779793928,4.66864974641035));
#9190=CARTESIAN_POINT('Ctrl Pts',(6.70820868996388,0.557592736564421,4.80642809587619));
#9191=CARTESIAN_POINT('Ctrl Pts',(6.71380490830661,0.632807795501951,4.93556873282767));
#9192=CARTESIAN_POINT('Ctrl Pts',(6.71731244248601,0.666836920456702,5.02812885948168));
#9193=CARTESIAN_POINT('Ctrl Pts',(6.71917582310349,0.680406120596861,5.07513188532028));
#9194=CARTESIAN_POINT('Ctrl Pts',(6.72133213271133,0.6909093875254,5.1233938812218));
#9195=CARTESIAN_POINT('Ctrl Pts',(6.72306773259333,0.700241175081311,5.19054637990825));
#9196=CARTESIAN_POINT('Ctrl Pts',(6.72619261442483,0.703178325652587,5.2668476785023));
#9197=CARTESIAN_POINT('Ctrl Pts',(6.7381664251681,0.689514001675121,5.39852659753196));
#9198=CARTESIAN_POINT('Ctrl Pts',(6.75463925550615,0.618247264838858,5.61826960075177));
#9199=CARTESIAN_POINT('Ctrl Pts',(6.77590827674278,0.436470460186145,5.81941560675087));
#9200=CARTESIAN_POINT('Ctrl Pts',(6.79564326301645,0.196280809931693,5.9247163591309));
#9201=CARTESIAN_POINT('Ctrl Pts',(6.81582644522033,-0.0629302930494358,
5.96025522192144));
#9202=CARTESIAN_POINT('Ctrl Pts',(6.84069654900574,-0.38497400844017,5.86555713916006));
#9203=CARTESIAN_POINT('Ctrl Pts',(6.86947638412051,-0.640427331596973,5.57601421543896));
#9204=CARTESIAN_POINT('Ctrl Pts',(6.89697365083529,-0.710923798883682,5.21615884811777));
#9205=CARTESIAN_POINT('Ctrl Pts',(6.92329898795441,-0.605777386429107,4.88177837844538));
#9206=CARTESIAN_POINT('Ctrl Pts',(6.94951107797999,-0.354456178032768,4.63917675459059));
#9207=CARTESIAN_POINT('Ctrl Pts',(6.97563701108018,-0.0190898795841548,
4.54673256040166));
#9208=CARTESIAN_POINT('Ctrl Pts',(7.00166306815893,0.318420157020357,4.6254869521555));
#9209=CARTESIAN_POINT('Ctrl Pts',(7.02543388521809,0.554722542828515,4.83645416115326));
#9210=CARTESIAN_POINT('Ctrl Pts',(7.04697773806416,0.666084600719225,5.09617679024369));
#9211=CARTESIAN_POINT('Ctrl Pts',(7.07276315353201,0.678427725557665,5.43526847721852));
#9212=CARTESIAN_POINT('Ctrl Pts',(7.10058962059944,0.484472501752673,5.76690932949108));
#9213=CARTESIAN_POINT('Ctrl Pts',(7.13043692169364,0.120638399689201,5.92825455906627));
#9214=CARTESIAN_POINT('Ctrl Pts',(7.1559402685194,-0.217537459809761,5.90145833585114));
#9215=CARTESIAN_POINT('Ctrl Pts',(7.17606991375773,-0.442156866353605,5.75500273582888));
#9216=CARTESIAN_POINT('Ctrl Pts',(7.1908732639631,-0.55830610816236,5.60220615030058));
#9217=CARTESIAN_POINT('Ctrl Pts',(7.20354845498638,-0.631705810891337,5.45532626907927));
#9218=CARTESIAN_POINT('Ctrl Pts',(7.22569553162755,-0.685810607871027,5.1691057765553));
#9219=CARTESIAN_POINT('Ctrl Pts',(7.25723947880328,-0.525122526582691,4.7636055764722));
#9220=CARTESIAN_POINT('Ctrl Pts',(7.29495362238925,-0.053457135933399,4.53870854204931));
#9221=CARTESIAN_POINT('Ctrl Pts',(7.33254246780218,0.443142598581714,4.69413693222259));
#9222=CARTESIAN_POINT('Ctrl Pts',(7.37001978026861,0.701091243696442,5.14423427781829));
#9223=CARTESIAN_POINT('Ctrl Pts',(7.40739968824424,0.584157721738047,5.64880921553006));
#9224=CARTESIAN_POINT('Ctrl Pts',(7.43848048896546,0.228011772623945,5.88938664283398));
#9225=CARTESIAN_POINT('Ctrl Pts',(7.46331103237168,-0.0982454758707846,
5.89962806423389));
#9226=CARTESIAN_POINT('Ctrl Pts',(7.48398628613683,-0.354294590444537,5.80983193950292));
#9227=CARTESIAN_POINT('Ctrl Pts',(7.50671008387199,-0.570451156260486,5.59791253961241));
#9228=CARTESIAN_POINT('Ctrl Pts',(7.53148051029953,-0.667000675030891,5.28247942808214));
#9229=CARTESIAN_POINT('Ctrl Pts',(7.55211030997723,-0.61172699107091,5.01340213779963));
#9230=CARTESIAN_POINT('Ctrl Pts',(7.56860908294787,-0.494743373007304,4.8335093105102));
#9231=CARTESIAN_POINT('Ctrl Pts',(7.58510523358743,-0.337168872759663,4.68756299395369));
#9232=CARTESIAN_POINT('Ctrl Pts',(7.60572192687897,-0.0819019612031444,
4.58805237352457));
#9233=CARTESIAN_POINT('Ctrl Pts',(7.63458408889819,0.300170619986696,4.63555033917682));
#9234=CARTESIAN_POINT('Ctrl Pts',(7.66138943476793,0.571053603076512,4.88796924826266));
#9235=CARTESIAN_POINT('Ctrl Pts',(7.68614446458683,0.653366892065435,5.20295921197447));
#9236=CARTESIAN_POINT('Ctrl Pts',(7.71090979818012,0.617991353788974,5.52603673989692));
#9237=CARTESIAN_POINT('Ctrl Pts',(7.74189055099461,0.350623503322525,5.86154592695952));
#9238=CARTESIAN_POINT('Ctrl Pts',(7.77601859800523,-0.116495965826188,5.93082813098408));
#9239=CARTESIAN_POINT('Ctrl Pts',(7.80709414997369,-0.481412412605556,5.72789933690448));
#9240=CARTESIAN_POINT('Ctrl Pts',(7.83510698559819,-0.663163478596285,5.39892523906655));
#9241=CARTESIAN_POINT('Ctrl Pts',(7.85615485977222,-0.647079306054213,5.11675578479515));
#9242=CARTESIAN_POINT('Ctrl Pts',(7.87020459706828,-0.574886104874813,4.94990033899215));
#9243=CARTESIAN_POINT('Ctrl Pts',(7.87723312367712,-0.527583060020924,4.87226677612988));
#9244=CARTESIAN_POINT('Ctrl Pts',(7.88426540124521,-0.469793796464868,4.80191051673322));
#9245=CARTESIAN_POINT('Ctrl Pts',(7.89521047892777,-0.365529336701908,4.7063343213378));
#9246=CARTESIAN_POINT('Ctrl Pts',(7.91634048666751,-0.120063962380262,4.57508935662309));
#9247=CARTESIAN_POINT('Ctrl Pts',(7.94458071734118,0.268642859242054,4.60441791433467));
#9248=CARTESIAN_POINT('Ctrl Pts',(7.97605533596052,0.584027938453731,4.88737223927164));
#9249=CARTESIAN_POINT('Ctrl Pts',(8.00446254702578,0.689638060716412,5.2531749302134));
#9250=CARTESIAN_POINT('Ctrl Pts',(8.03295521872146,0.583958260807566,5.62109535966095));
#9251=CARTESIAN_POINT('Ctrl Pts',(8.06153860386915,0.297951770638925,5.87686527268886));
#9252=CARTESIAN_POINT('Ctrl Pts',(8.09021776831132,-0.0816004700383042,
5.94171985993802));
#9253=CARTESIAN_POINT('Ctrl Pts',(8.11899761019108,-0.438736741574054,5.7941606881638));
#9254=CARTESIAN_POINT('Ctrl Pts',(8.14788283876726,-0.66350439566471,5.47812772009615));
#9255=CARTESIAN_POINT('Ctrl Pts',(8.17687795851733,-0.6858207744463,5.08946678694388));
#9256=CARTESIAN_POINT('Ctrl Pts',(8.20598727446933,-0.497249207778955,4.74714184053921));
#9257=CARTESIAN_POINT('Ctrl Pts',(8.23521486961617,-0.154093127286878,4.55679071733693));
#9258=CARTESIAN_POINT('Ctrl Pts',(8.26456461818433,0.239380388009074,4.57821827016813));
#9259=CARTESIAN_POINT('Ctrl Pts',(8.29404014876887,0.562549974717286,4.80663318942082));
#9260=CARTESIAN_POINT('Ctrl Pts',(8.32364486518472,0.715391021033525,5.17354565176085));
#9261=CARTESIAN_POINT('Ctrl Pts',(8.35338192623768,0.649330974858417,5.56731319891309));
#9262=CARTESIAN_POINT('Ctrl Pts',(8.38325424070601,0.382790348017333,5.86693311075399));
#9263=CARTESIAN_POINT('Ctrl Pts',(8.41326446409716,-0.00419505000370753,
5.97947359705855));
#9264=CARTESIAN_POINT('Ctrl Pts',(8.43838990507217,-0.328427739096548,5.88675138216907));
#9265=CARTESIAN_POINT('Ctrl Pts',(8.45856147729175,-0.529480619639225,5.71722997945441));
#9266=CARTESIAN_POINT('Ctrl Pts',(8.47765754585014,-0.668434606896997,5.5107649981822));
#9267=CARTESIAN_POINT('Ctrl Pts',(8.50076123794206,-0.730336170493974,5.20937619755011));
#9268=CARTESIAN_POINT('Ctrl Pts',(8.52792461605616,-0.624513035959022,4.86362366838459));
#9269=CARTESIAN_POINT('Ctrl Pts',(8.5529308052989,-0.386883838373545,4.6302289824672));
#9270=CARTESIAN_POINT('Ctrl Pts',(8.57574894485481,-0.104298108040022,4.53121501380808));
#9271=CARTESIAN_POINT('Ctrl Pts',(8.6032187287894,0.256675810750089,4.54226136093568));
#9272=CARTESIAN_POINT('Ctrl Pts',(8.63772155686955,0.652405168310869,4.80876975888547));
#9273=CARTESIAN_POINT('Ctrl Pts',(8.67939097890975,0.783030401351032,5.37140034010679));
#9274=CARTESIAN_POINT('Ctrl Pts',(8.72132656843746,0.49495090614558,5.87513455402037));
#9275=CARTESIAN_POINT('Ctrl Pts',(8.76352759225084,-0.0628635021467805,
6.05013777316939));
#9276=CARTESIAN_POINT('Ctrl Pts',(8.79891493140875,-0.504716359285686,5.83905645697925));
#9277=CARTESIAN_POINT('Ctrl Pts',(8.82735545219243,-0.703159459402567,5.5227896978014));
#9278=CARTESIAN_POINT('Ctrl Pts',(8.85588259535385,-0.776061781005718,5.15482469233793));
#9279=CARTESIAN_POINT('Ctrl Pts',(8.88692644387892,-0.621492770362474,4.75483748689365));
#9280=CARTESIAN_POINT('Ctrl Pts',(8.92052297991862,-0.245496738926199,4.51104937209089));
#9281=CARTESIAN_POINT('Ctrl Pts',(8.94943095663315,0.137693585331708,4.48033145317999));
#9282=CARTESIAN_POINT('Ctrl Pts',(8.97965767299615,0.505669735297425,4.64426980471776));
#9283=CARTESIAN_POINT('Ctrl Pts',(9.01121604967911,0.752482582266742,4.98850418901732));
#9284=CARTESIAN_POINT('Ctrl Pts',(9.04412144632782,0.779510405814253,5.42959222113123));
#9285=CARTESIAN_POINT('Ctrl Pts',(9.07715711994043,0.566889248726445,5.81885947968755));
#9286=CARTESIAN_POINT('Ctrl Pts',(9.11031735538565,0.178292209075846,6.0362617860296));
#9287=CARTESIAN_POINT('Ctrl Pts',(9.14360253722173,-0.268079437778697,6.01351727669282));
#9288=CARTESIAN_POINT('Ctrl Pts',(9.17699734546285,-0.635285771434068,5.75590592911153));
#9289=CARTESIAN_POINT('Ctrl Pts',(9.21051983173094,-0.809796215592389,5.34095865996421));
#9290=CARTESIAN_POINT('Ctrl Pts',(9.24411094986739,-0.736619369561702,4.89534022537719));
#9291=CARTESIAN_POINT('Ctrl Pts',(9.27788074499435,-0.436616793358521,4.55570108560577));
#9292=CARTESIAN_POINT('Ctrl Pts',(9.30594116368128,-0.0733420592947115,
4.44897069772665));
#9293=CARTESIAN_POINT('Ctrl Pts',(9.328680473888,0.218704827060702,4.48901682699427));
#9294=CARTESIAN_POINT('Ctrl Pts',(9.35089495840618,0.489065381509997,4.60762593183536));
#9295=CARTESIAN_POINT('Ctrl Pts',(9.37480209610635,0.693278005812641,4.83358316838714));
#9296=CARTESIAN_POINT('Ctrl Pts',(9.39327740184756,0.773205179450414,5.08031011736591));
#9297=CARTESIAN_POINT('Ctrl Pts',(9.40667901531909,0.788514168138214,5.22730031946394));
#9298=CARTESIAN_POINT('Ctrl Pts',(9.41035265957923,0.785191918284243,5.31605807341251));
#9299=CARTESIAN_POINT('Ctrl Pts',(9.41223809751033,0.774762970480976,5.39019446309586));
#9300=CARTESIAN_POINT('Ctrl Pts',(9.4146591021466,0.763068583364469,5.44423938068532));
#9301=CARTESIAN_POINT('Ctrl Pts',(9.4167523666832,0.747778571803171,5.49710428778674));
#9302=CARTESIAN_POINT('Ctrl Pts',(9.42068446598339,0.709658392601865,5.60083098220104));
#9303=CARTESIAN_POINT('Ctrl Pts',(9.42695148511213,0.625399217361514,5.74546397737963));
#9304=CARTESIAN_POINT('Ctrl Pts',(9.4350913459169,0.463897848898915,5.89967743034001));
#9305=CARTESIAN_POINT('Ctrl Pts',(9.44332988824765,0.265871334396363,6.00323600320908));
#9306=CARTESIAN_POINT('Ctrl Pts',(9.45153347644623,0.0468430344411857,6.04773546710682));
#9307=CARTESIAN_POINT('Ctrl Pts',(9.46250188685132,-0.250556076226033,6.02429177474909));
#9308=CARTESIAN_POINT('Ctrl Pts',(9.47620737800529,-0.587650060167328,5.84004639330421));
#9309=CARTESIAN_POINT('Ctrl Pts',(9.49268366719886,-0.81241635296479,5.43659555942134));
#9310=CARTESIAN_POINT('Ctrl Pts',(9.50917374900608,-0.787865415172378,4.9752477474741));
#9311=CARTESIAN_POINT('Ctrl Pts',(9.52568233488031,-0.521201295938573,4.59717415541696));
#9312=CARTESIAN_POINT('Ctrl Pts',(9.5422061736552,-0.0937383220535699,4.41946428983354));
#9313=CARTESIAN_POINT('Ctrl Pts',(9.55874735915243,0.363109547604185,4.49620059730279));
#9314=CARTESIAN_POINT('Ctrl Pts',(9.57529830568314,0.709172657538417,4.80516325810888));
#9315=CARTESIAN_POINT('Ctrl Pts',(9.58634758255215,0.794862864598598,5.10196837702893));
#9316=CARTESIAN_POINT('Ctrl Pts',(9.59186670251247,0.79488293160754,5.25103156499837));
#9317=CARTESIAN_POINT('',(6.55994469204049,0.719709328495781,5.24703997894806));
#9318=CARTESIAN_POINT('Origin',(6.48,0.72,5.25));
#9319=CARTESIAN_POINT('',(9.59186670251247,0.79488293160754,5.25103156499837));
#9320=CARTESIAN_POINT('Ctrl Pts',(6.55994469204049,0.719709328495781,5.24703997894806));
#9321=CARTESIAN_POINT('Ctrl Pts',(6.56494552765653,0.719691145920131,5.38210508200347));
#9322=CARTESIAN_POINT('Ctrl Pts',(6.57494016333875,0.642089168505731,5.65058609468785));
#9323=CARTESIAN_POINT('Ctrl Pts',(6.58989438616266,0.32941528595114,5.9296313569664));
#9324=CARTESIAN_POINT('Ctrl Pts',(6.60481477071411,-0.0827797453005289,
5.99886361370576));
#9325=CARTESIAN_POINT('Ctrl Pts',(6.61969980345594,-0.467619845512657,5.83844773036597));
#9326=CARTESIAN_POINT('Ctrl Pts',(6.63454965842308,-0.707639327219362,5.49857002500469));
#9327=CARTESIAN_POINT('Ctrl Pts',(6.64936061260475,-0.729495436544756,5.0840660001111));
#9328=CARTESIAN_POINT('Ctrl Pts',(6.66414030226907,-0.527844751315962,4.72224444577032));
#9329=CARTESIAN_POINT('Ctrl Pts',(6.67641810037933,-0.225796647591973,4.55722222010489));
#9330=CARTESIAN_POINT('Ctrl Pts',(6.68623494447203,0.0403746271135037,4.5362580751361));
#9331=CARTESIAN_POINT('Ctrl Pts',(6.69357256905876,0.236291461979514,4.57606849800983));
#9332=CARTESIAN_POINT('Ctrl Pts',(6.70093718034598,0.413303779793928,4.66864974641035));
#9333=CARTESIAN_POINT('Ctrl Pts',(6.70820868996388,0.557592736564421,4.80642809587619));
#9334=CARTESIAN_POINT('Ctrl Pts',(6.71380490830661,0.632807795501951,4.93556873282767));
#9335=CARTESIAN_POINT('Ctrl Pts',(6.71731244248601,0.666836920456702,5.02812885948168));
#9336=CARTESIAN_POINT('Ctrl Pts',(6.71917582310349,0.680406120596861,5.07513188532028));
#9337=CARTESIAN_POINT('Ctrl Pts',(6.72133213271133,0.6909093875254,5.1233938812218));
#9338=CARTESIAN_POINT('Ctrl Pts',(6.72306773259333,0.700241175081311,5.19054637990825));
#9339=CARTESIAN_POINT('Ctrl Pts',(6.72619261442483,0.703178325652587,5.2668476785023));
#9340=CARTESIAN_POINT('Ctrl Pts',(6.7381664251681,0.689514001675121,5.39852659753196));
#9341=CARTESIAN_POINT('Ctrl Pts',(6.75463925550615,0.618247264838858,5.61826960075177));
#9342=CARTESIAN_POINT('Ctrl Pts',(6.77590827674278,0.436470460186145,5.81941560675087));
#9343=CARTESIAN_POINT('Ctrl Pts',(6.79564326301645,0.196280809931693,5.9247163591309));
#9344=CARTESIAN_POINT('Ctrl Pts',(6.81582644522033,-0.0629302930494358,
5.96025522192144));
#9345=CARTESIAN_POINT('Ctrl Pts',(6.84069654900574,-0.38497400844017,5.86555713916006));
#9346=CARTESIAN_POINT('Ctrl Pts',(6.86947638412051,-0.640427331596973,5.57601421543896));
#9347=CARTESIAN_POINT('Ctrl Pts',(6.89697365083529,-0.710923798883682,5.21615884811777));
#9348=CARTESIAN_POINT('Ctrl Pts',(6.92329898795441,-0.605777386429107,4.88177837844538));
#9349=CARTESIAN_POINT('Ctrl Pts',(6.94951107797999,-0.354456178032768,4.63917675459059));
#9350=CARTESIAN_POINT('Ctrl Pts',(6.97563701108018,-0.0190898795841548,
4.54673256040166));
#9351=CARTESIAN_POINT('Ctrl Pts',(7.00166306815893,0.318420157020357,4.6254869521555));
#9352=CARTESIAN_POINT('Ctrl Pts',(7.02543388521809,0.554722542828515,4.83645416115326));
#9353=CARTESIAN_POINT('Ctrl Pts',(7.04697773806416,0.666084600719225,5.09617679024369));
#9354=CARTESIAN_POINT('Ctrl Pts',(7.07276315353201,0.678427725557665,5.43526847721852));
#9355=CARTESIAN_POINT('Ctrl Pts',(7.10058962059944,0.484472501752673,5.76690932949108));
#9356=CARTESIAN_POINT('Ctrl Pts',(7.13043692169364,0.120638399689201,5.92825455906627));
#9357=CARTESIAN_POINT('Ctrl Pts',(7.1559402685194,-0.217537459809761,5.90145833585114));
#9358=CARTESIAN_POINT('Ctrl Pts',(7.17606991375773,-0.442156866353605,5.75500273582888));
#9359=CARTESIAN_POINT('Ctrl Pts',(7.1908732639631,-0.55830610816236,5.60220615030058));
#9360=CARTESIAN_POINT('Ctrl Pts',(7.20354845498638,-0.631705810891337,5.45532626907927));
#9361=CARTESIAN_POINT('Ctrl Pts',(7.22569553162755,-0.685810607871027,5.1691057765553));
#9362=CARTESIAN_POINT('Ctrl Pts',(7.25723947880328,-0.525122526582691,4.7636055764722));
#9363=CARTESIAN_POINT('Ctrl Pts',(7.29495362238925,-0.053457135933399,4.53870854204931));
#9364=CARTESIAN_POINT('Ctrl Pts',(7.33254246780218,0.443142598581714,4.69413693222259));
#9365=CARTESIAN_POINT('Ctrl Pts',(7.37001978026861,0.701091243696442,5.14423427781829));
#9366=CARTESIAN_POINT('Ctrl Pts',(7.40739968824424,0.584157721738047,5.64880921553006));
#9367=CARTESIAN_POINT('Ctrl Pts',(7.43848048896546,0.228011772623945,5.88938664283398));
#9368=CARTESIAN_POINT('Ctrl Pts',(7.46331103237168,-0.0982454758707846,
5.89962806423389));
#9369=CARTESIAN_POINT('Ctrl Pts',(7.48398628613683,-0.354294590444537,5.80983193950292));
#9370=CARTESIAN_POINT('Ctrl Pts',(7.50671008387199,-0.570451156260486,5.59791253961241));
#9371=CARTESIAN_POINT('Ctrl Pts',(7.53148051029953,-0.667000675030891,5.28247942808214));
#9372=CARTESIAN_POINT('Ctrl Pts',(7.55211030997723,-0.61172699107091,5.01340213779963));
#9373=CARTESIAN_POINT('Ctrl Pts',(7.56860908294787,-0.494743373007304,4.8335093105102));
#9374=CARTESIAN_POINT('Ctrl Pts',(7.58510523358743,-0.337168872759663,4.68756299395369));
#9375=CARTESIAN_POINT('Ctrl Pts',(7.60572192687897,-0.0819019612031444,
4.58805237352457));
#9376=CARTESIAN_POINT('Ctrl Pts',(7.63458408889819,0.300170619986696,4.63555033917682));
#9377=CARTESIAN_POINT('Ctrl Pts',(7.66138943476793,0.571053603076512,4.88796924826266));
#9378=CARTESIAN_POINT('Ctrl Pts',(7.68614446458683,0.653366892065435,5.20295921197447));
#9379=CARTESIAN_POINT('Ctrl Pts',(7.71090979818012,0.617991353788974,5.52603673989692));
#9380=CARTESIAN_POINT('Ctrl Pts',(7.74189055099461,0.350623503322525,5.86154592695952));
#9381=CARTESIAN_POINT('Ctrl Pts',(7.77601859800523,-0.116495965826188,5.93082813098408));
#9382=CARTESIAN_POINT('Ctrl Pts',(7.80709414997369,-0.481412412605556,5.72789933690448));
#9383=CARTESIAN_POINT('Ctrl Pts',(7.83510698559819,-0.663163478596285,5.39892523906655));
#9384=CARTESIAN_POINT('Ctrl Pts',(7.85615485977222,-0.647079306054213,5.11675578479515));
#9385=CARTESIAN_POINT('Ctrl Pts',(7.87020459706828,-0.574886104874813,4.94990033899215));
#9386=CARTESIAN_POINT('Ctrl Pts',(7.87723312367712,-0.527583060020924,4.87226677612988));
#9387=CARTESIAN_POINT('Ctrl Pts',(7.88426540124521,-0.469793796464868,4.80191051673322));
#9388=CARTESIAN_POINT('Ctrl Pts',(7.89521047892777,-0.365529336701908,4.7063343213378));
#9389=CARTESIAN_POINT('Ctrl Pts',(7.91634048666751,-0.120063962380262,4.57508935662309));
#9390=CARTESIAN_POINT('Ctrl Pts',(7.94458071734118,0.268642859242054,4.60441791433467));
#9391=CARTESIAN_POINT('Ctrl Pts',(7.97605533596052,0.584027938453731,4.88737223927164));
#9392=CARTESIAN_POINT('Ctrl Pts',(8.00446254702578,0.689638060716412,5.2531749302134));
#9393=CARTESIAN_POINT('Ctrl Pts',(8.03295521872146,0.583958260807566,5.62109535966095));
#9394=CARTESIAN_POINT('Ctrl Pts',(8.06153860386915,0.297951770638925,5.87686527268886));
#9395=CARTESIAN_POINT('Ctrl Pts',(8.09021776831132,-0.0816004700383042,
5.94171985993802));
#9396=CARTESIAN_POINT('Ctrl Pts',(8.11899761019108,-0.438736741574054,5.7941606881638));
#9397=CARTESIAN_POINT('Ctrl Pts',(8.14788283876726,-0.66350439566471,5.47812772009615));
#9398=CARTESIAN_POINT('Ctrl Pts',(8.17687795851733,-0.6858207744463,5.08946678694388));
#9399=CARTESIAN_POINT('Ctrl Pts',(8.20598727446933,-0.497249207778955,4.74714184053921));
#9400=CARTESIAN_POINT('Ctrl Pts',(8.23521486961617,-0.154093127286878,4.55679071733693));
#9401=CARTESIAN_POINT('Ctrl Pts',(8.26456461818433,0.239380388009074,4.57821827016813));
#9402=CARTESIAN_POINT('Ctrl Pts',(8.29404014876887,0.562549974717286,4.80663318942082));
#9403=CARTESIAN_POINT('Ctrl Pts',(8.32364486518472,0.715391021033525,5.17354565176085));
#9404=CARTESIAN_POINT('Ctrl Pts',(8.35338192623768,0.649330974858417,5.56731319891309));
#9405=CARTESIAN_POINT('Ctrl Pts',(8.38325424070601,0.382790348017333,5.86693311075399));
#9406=CARTESIAN_POINT('Ctrl Pts',(8.41326446409716,-0.00419505000370753,
5.97947359705855));
#9407=CARTESIAN_POINT('Ctrl Pts',(8.43838990507217,-0.328427739096548,5.88675138216907));
#9408=CARTESIAN_POINT('Ctrl Pts',(8.45856147729175,-0.529480619639225,5.71722997945441));
#9409=CARTESIAN_POINT('Ctrl Pts',(8.47765754585014,-0.668434606896997,5.5107649981822));
#9410=CARTESIAN_POINT('Ctrl Pts',(8.50076123794206,-0.730336170493974,5.20937619755011));
#9411=CARTESIAN_POINT('Ctrl Pts',(8.52792461605616,-0.624513035959022,4.86362366838459));
#9412=CARTESIAN_POINT('Ctrl Pts',(8.5529308052989,-0.386883838373545,4.6302289824672));
#9413=CARTESIAN_POINT('Ctrl Pts',(8.57574894485481,-0.104298108040022,4.53121501380808));
#9414=CARTESIAN_POINT('Ctrl Pts',(8.6032187287894,0.256675810750089,4.54226136093568));
#9415=CARTESIAN_POINT('Ctrl Pts',(8.63772155686955,0.652405168310869,4.80876975888547));
#9416=CARTESIAN_POINT('Ctrl Pts',(8.67939097890975,0.783030401351032,5.37140034010679));
#9417=CARTESIAN_POINT('Ctrl Pts',(8.72132656843746,0.49495090614558,5.87513455402037));
#9418=CARTESIAN_POINT('Ctrl Pts',(8.76352759225084,-0.0628635021467805,
6.05013777316939));
#9419=CARTESIAN_POINT('Ctrl Pts',(8.79891493140875,-0.504716359285686,5.83905645697925));
#9420=CARTESIAN_POINT('Ctrl Pts',(8.82735545219243,-0.703159459402567,5.5227896978014));
#9421=CARTESIAN_POINT('Ctrl Pts',(8.85588259535385,-0.776061781005718,5.15482469233793));
#9422=CARTESIAN_POINT('Ctrl Pts',(8.88692644387892,-0.621492770362474,4.75483748689365));
#9423=CARTESIAN_POINT('Ctrl Pts',(8.92052297991862,-0.245496738926199,4.51104937209089));
#9424=CARTESIAN_POINT('Ctrl Pts',(8.94943095663315,0.137693585331708,4.48033145317999));
#9425=CARTESIAN_POINT('Ctrl Pts',(8.97965767299615,0.505669735297425,4.64426980471776));
#9426=CARTESIAN_POINT('Ctrl Pts',(9.01121604967911,0.752482582266742,4.98850418901732));
#9427=CARTESIAN_POINT('Ctrl Pts',(9.04412144632782,0.779510405814253,5.42959222113123));
#9428=CARTESIAN_POINT('Ctrl Pts',(9.07715711994043,0.566889248726445,5.81885947968755));
#9429=CARTESIAN_POINT('Ctrl Pts',(9.11031735538565,0.178292209075846,6.0362617860296));
#9430=CARTESIAN_POINT('Ctrl Pts',(9.14360253722173,-0.268079437778697,6.01351727669282));
#9431=CARTESIAN_POINT('Ctrl Pts',(9.17699734546285,-0.635285771434068,5.75590592911153));
#9432=CARTESIAN_POINT('Ctrl Pts',(9.21051983173094,-0.809796215592389,5.34095865996421));
#9433=CARTESIAN_POINT('Ctrl Pts',(9.24411094986739,-0.736619369561702,4.89534022537719));
#9434=CARTESIAN_POINT('Ctrl Pts',(9.27788074499435,-0.436616793358521,4.55570108560577));
#9435=CARTESIAN_POINT('Ctrl Pts',(9.30594116368128,-0.0733420592947115,
4.44897069772665));
#9436=CARTESIAN_POINT('Ctrl Pts',(9.328680473888,0.218704827060702,4.48901682699427));
#9437=CARTESIAN_POINT('Ctrl Pts',(9.35089495840618,0.489065381509997,4.60762593183536));
#9438=CARTESIAN_POINT('Ctrl Pts',(9.37480209610635,0.693278005812641,4.83358316838714));
#9439=CARTESIAN_POINT('Ctrl Pts',(9.39327740184756,0.773205179450414,5.08031011736591));
#9440=CARTESIAN_POINT('Ctrl Pts',(9.40667901531909,0.788514168138214,5.22730031946394));
#9441=CARTESIAN_POINT('Ctrl Pts',(9.41035265957923,0.785191918284243,5.31605807341251));
#9442=CARTESIAN_POINT('Ctrl Pts',(9.41223809751033,0.774762970480976,5.39019446309586));
#9443=CARTESIAN_POINT('Ctrl Pts',(9.4146591021466,0.763068583364469,5.44423938068532));
#9444=CARTESIAN_POINT('Ctrl Pts',(9.4167523666832,0.747778571803171,5.49710428778674));
#9445=CARTESIAN_POINT('Ctrl Pts',(9.42068446598339,0.709658392601865,5.60083098220104));
#9446=CARTESIAN_POINT('Ctrl Pts',(9.42695148511213,0.625399217361514,5.74546397737963));
#9447=CARTESIAN_POINT('Ctrl Pts',(9.4350913459169,0.463897848898915,5.89967743034001));
#9448=CARTESIAN_POINT('Ctrl Pts',(9.44332988824765,0.265871334396363,6.00323600320908));
#9449=CARTESIAN_POINT('Ctrl Pts',(9.45153347644623,0.0468430344411857,6.04773546710682));
#9450=CARTESIAN_POINT('Ctrl Pts',(9.46250188685132,-0.250556076226033,6.02429177474909));
#9451=CARTESIAN_POINT('Ctrl Pts',(9.47620737800529,-0.587650060167328,5.84004639330421));
#9452=CARTESIAN_POINT('Ctrl Pts',(9.49268366719886,-0.81241635296479,5.43659555942134));
#9453=CARTESIAN_POINT('Ctrl Pts',(9.50917374900608,-0.787865415172378,4.9752477474741));
#9454=CARTESIAN_POINT('Ctrl Pts',(9.52568233488031,-0.521201295938573,4.59717415541696));
#9455=CARTESIAN_POINT('Ctrl Pts',(9.5422061736552,-0.0937383220535699,4.41946428983354));
#9456=CARTESIAN_POINT('Ctrl Pts',(9.55874735915243,0.363109547604185,4.49620059730279));
#9457=CARTESIAN_POINT('Ctrl Pts',(9.57529830568314,0.709172657538417,4.80516325810888));
#9458=CARTESIAN_POINT('Ctrl Pts',(9.58634758255215,0.794862864598598,5.10196837702893));
#9459=CARTESIAN_POINT('Ctrl Pts',(9.59186670251247,0.79488293160754,5.25103156499837));
#9460=CARTESIAN_POINT('Origin',(9.61999999999987,0.720000000000002,5.25));
#9461=CARTESIAN_POINT('Origin',(9.61999999999987,0.720000000000002,5.25));
#9462=CARTESIAN_POINT('Origin',(6.48,0.72,5.25));
#9463=CARTESIAN_POINT('',(0.,0.,0.));
#9464=CARTESIAN_POINT('Origin',(0.9,0.,1.4));
#9465=CARTESIAN_POINT('',(0.988888264668966,0.25,1.4));
#9466=CARTESIAN_POINT('',(1.02,-1.18386380373883E-17,1.65));
#9467=CARTESIAN_POINT('Ctrl Pts',(0.988888264668966,0.25,1.4));
#9468=CARTESIAN_POINT('Ctrl Pts',(0.988888264668966,0.25,1.43153139415882));
#9469=CARTESIAN_POINT('Ctrl Pts',(0.990553370646674,0.243672048431404,1.46507214966317));
#9470=CARTESIAN_POINT('Ctrl Pts',(0.996491737296663,0.218119830014375,1.52662620974954));
#9471=CARTESIAN_POINT('Ctrl Pts',(1.00067109353237,0.198902128206072,1.5546512623872));
#9472=CARTESIAN_POINT('Ctrl Pts',(1.00845756932386,0.154654113568716,1.59889927702456));
#9473=CARTESIAN_POINT('Ctrl Pts',(1.01258144235289,0.126627870945253,1.61811920309393));
#9474=CARTESIAN_POINT('Ctrl Pts',(1.0183917429657,0.065069600391363,1.64367304400768));
#9475=CARTESIAN_POINT('Ctrl Pts',(1.02,0.031527330883376,1.65));
#9476=CARTESIAN_POINT('Ctrl Pts',(1.02,2.77555756156289E-17,1.65));
#9477=CARTESIAN_POINT('Ctrl Pts',(1.02,6.93889390390723E-18,1.65));
#9478=CARTESIAN_POINT('Ctrl Pts',(1.02,-0.031527330883376,1.65));
#9479=CARTESIAN_POINT('Ctrl Pts',(1.0183917429657,-0.065069600391363,1.64367304400768));
#9480=CARTESIAN_POINT('Ctrl Pts',(1.01258144235289,-0.126627870945253,1.61811920309393));
#9481=CARTESIAN_POINT('Ctrl Pts',(1.00845756932386,-0.154654113568716,1.59889927702456));
#9482=CARTESIAN_POINT('Ctrl Pts',(1.00067109353237,-0.198902128206072,1.5546512623872));
#9483=CARTESIAN_POINT('Ctrl Pts',(0.996491737296663,-0.218119830014375,
1.52662620974954));
#9484=CARTESIAN_POINT('Ctrl Pts',(0.990553370646674,-0.243672048431404,
1.46507214966317));
#9485=CARTESIAN_POINT('Ctrl Pts',(0.988888264668967,-0.25,1.43153139415882));
#9486=CARTESIAN_POINT('Ctrl Pts',(0.988888264668967,-0.25,1.36846860584118));
#9487=CARTESIAN_POINT('Ctrl Pts',(0.990553370646674,-0.243672048431404,
1.33492785033683));
#9488=CARTESIAN_POINT('Ctrl Pts',(0.996491737296663,-0.218119830014375,
1.27337379025046));
#9489=CARTESIAN_POINT('Ctrl Pts',(1.00067109353237,-0.198902128206072,1.2453487376128));
#9490=CARTESIAN_POINT('Ctrl Pts',(1.00845756932386,-0.154654113568716,1.20110072297544));
#9491=CARTESIAN_POINT('Ctrl Pts',(1.01258144235289,-0.126627870945254,1.18188079690607));
#9492=CARTESIAN_POINT('Ctrl Pts',(1.0183917429657,-0.0650696003913633,1.15632695599232));
#9493=CARTESIAN_POINT('Ctrl Pts',(1.02,-0.0315273308833761,1.15));
#9494=CARTESIAN_POINT('Ctrl Pts',(1.02,0.0315273308833759,1.15));
#9495=CARTESIAN_POINT('Ctrl Pts',(1.0183917429657,0.065069600391363,1.15632695599232));
#9496=CARTESIAN_POINT('Ctrl Pts',(1.01258144235289,0.126627870945253,1.18188079690607));
#9497=CARTESIAN_POINT('Ctrl Pts',(1.00845756932386,0.154654113568716,1.20110072297544));
#9498=CARTESIAN_POINT('Ctrl Pts',(1.00067109353237,0.198902128206072,1.2453487376128));
#9499=CARTESIAN_POINT('Ctrl Pts',(0.996491737296663,0.218119830014375,1.27337379025046));
#9500=CARTESIAN_POINT('Ctrl Pts',(0.990553370646674,0.243672048431404,1.33492785033683));
#9501=CARTESIAN_POINT('Ctrl Pts',(0.988888264668967,0.25,1.36846860584118));
#9502=CARTESIAN_POINT('Ctrl Pts',(0.988888264668967,0.25,1.4));
#9503=CARTESIAN_POINT('',(3.,-3.06161699786838E-17,1.65));
#9504=CARTESIAN_POINT('',(0.9,-3.06161699786838E-17,1.65));
#9505=CARTESIAN_POINT('',(2.98956518577535,0.25,1.4));
#9506=CARTESIAN_POINT('Ctrl Pts',(2.98956518577535,0.25,1.4));
#9507=CARTESIAN_POINT('Ctrl Pts',(2.98956518577535,0.25,1.36859378633186));
#9508=CARTESIAN_POINT('Ctrl Pts',(2.99011104995181,0.24372047740942,1.33510417960069));
#9509=CARTESIAN_POINT('Ctrl Pts',(2.99208145165098,0.218202539734559,1.27351367328886));
#9510=CARTESIAN_POINT('Ctrl Pts',(2.99347740802958,0.198964922639276,1.245411532046));
#9511=CARTESIAN_POINT('Ctrl Pts',(2.99609686518216,0.154588504271054,1.20103511367778));
#9512=CARTESIAN_POINT('Ctrl Pts',(2.99749070376198,0.126486346986081,1.18179746841036));
#9513=CARTESIAN_POINT('Ctrl Pts',(2.99945625936844,0.0648957875009219,1.15627950921557));
#9514=CARTESIAN_POINT('Ctrl Pts',(3.,0.0314061622633416,1.15));
#9515=CARTESIAN_POINT('Ctrl Pts',(3.,-0.0314061622633416,1.15));
#9516=CARTESIAN_POINT('Ctrl Pts',(2.99945625936844,-0.0648957875009221,
1.15627950921557));
#9517=CARTESIAN_POINT('Ctrl Pts',(2.99749070376198,-0.126486346986081,1.18179746841036));
#9518=CARTESIAN_POINT('Ctrl Pts',(2.99609686518216,-0.154588504271054,1.20103511367778));
#9519=CARTESIAN_POINT('Ctrl Pts',(2.99347740802958,-0.198964922639276,1.245411532046));
#9520=CARTESIAN_POINT('Ctrl Pts',(2.99208145165098,-0.218202539734559,1.27351367328886));
#9521=CARTESIAN_POINT('Ctrl Pts',(2.99011104995181,-0.24372047740942,1.33510417960069));
#9522=CARTESIAN_POINT('Ctrl Pts',(2.98956518577535,-0.25,1.36859378633186));
#9523=CARTESIAN_POINT('Ctrl Pts',(2.98956518577535,-0.25,1.43140621366814));
#9524=CARTESIAN_POINT('Ctrl Pts',(2.99011104995181,-0.24372047740942,1.4648958203993));
#9525=CARTESIAN_POINT('Ctrl Pts',(2.99208145165098,-0.21820253973456,1.52648632671114));
#9526=CARTESIAN_POINT('Ctrl Pts',(2.99347740802958,-0.198964922639276,1.554588467954));
#9527=CARTESIAN_POINT('Ctrl Pts',(2.99609686518216,-0.154588504271054,1.59896488632222));
#9528=CARTESIAN_POINT('Ctrl Pts',(2.99749070376198,-0.126486346986082,1.61820253158964));
#9529=CARTESIAN_POINT('Ctrl Pts',(2.99945625936844,-0.0648957875009221,
1.64372049078443));
#9530=CARTESIAN_POINT('Ctrl Pts',(3.,-0.0314061622633417,1.65));
#9531=CARTESIAN_POINT('Ctrl Pts',(3.,-5.55111512312578E-17,1.65));
#9532=CARTESIAN_POINT('Ctrl Pts',(3.,-2.08166817117217E-17,1.65));
#9533=CARTESIAN_POINT('Ctrl Pts',(3.,0.0314061622633416,1.65));
#9534=CARTESIAN_POINT('Ctrl Pts',(2.99945625936844,0.0648957875009221,1.64372049078443));
#9535=CARTESIAN_POINT('Ctrl Pts',(2.99749070376198,0.126486346986081,1.61820253158964));
#9536=CARTESIAN_POINT('Ctrl Pts',(2.99609686518216,0.154588504271054,1.59896488632222));
#9537=CARTESIAN_POINT('Ctrl Pts',(2.99347740802958,0.198964922639276,1.554588467954));
#9538=CARTESIAN_POINT('Ctrl Pts',(2.99208145165098,0.218202539734559,1.52648632671114));
#9539=CARTESIAN_POINT('Ctrl Pts',(2.99011104995181,0.24372047740942,1.46489582039931));
#9540=CARTESIAN_POINT('Ctrl Pts',(2.98956518577535,0.25,1.43140621366814));
#9541=CARTESIAN_POINT('Ctrl Pts',(2.98956518577535,0.25,1.4));
#9542=CARTESIAN_POINT('Origin',(-1.23743686707646,-1.23743686707646,2.9));
#9543=CARTESIAN_POINT('',(-1.40243686707646,-1.23743686707646,2.9));
#9544=CARTESIAN_POINT('Origin',(-1.23743686707646,-1.23743686707646,2.9));
#9545=CARTESIAN_POINT('',(-1.40243686707646,-1.23743686707646,3.6));
#9546=CARTESIAN_POINT('',(-1.40243686707646,-1.23743686707646,2.9));
#9547=CARTESIAN_POINT('Origin',(-1.23743686707646,-1.23743686707646,3.6));
#9548=CARTESIAN_POINT('Origin',(-1.23743686707646,-1.23743686707646,2.9));
#9549=CARTESIAN_POINT('Origin',(-1.23743686707646,1.23743686707646,2.9));
#9550=CARTESIAN_POINT('',(-1.40243686707646,1.23743686707646,2.9));
#9551=CARTESIAN_POINT('Origin',(-1.23743686707646,1.23743686707646,2.9));
#9552=CARTESIAN_POINT('',(-1.40243686707646,1.23743686707646,3.6));
#9553=CARTESIAN_POINT('',(-1.40243686707646,1.23743686707646,2.9));
#9554=CARTESIAN_POINT('Origin',(-1.23743686707646,1.23743686707646,3.6));
#9555=CARTESIAN_POINT('Origin',(-1.23743686707646,1.23743686707646,2.9));
#9556=CARTESIAN_POINT('Origin',(1.23743686707646,1.23743686707646,2.9));
#9557=CARTESIAN_POINT('',(1.07243686707646,1.23743686707646,2.9));
#9558=CARTESIAN_POINT('Origin',(1.23743686707646,1.23743686707646,2.9));
#9559=CARTESIAN_POINT('',(1.07243686707646,1.23743686707646,3.6));
#9560=CARTESIAN_POINT('',(1.07243686707646,1.23743686707646,2.9));
#9561=CARTESIAN_POINT('Origin',(1.23743686707646,1.23743686707646,3.6));
#9562=CARTESIAN_POINT('Origin',(1.23743686707646,1.23743686707646,2.9));
#9563=CARTESIAN_POINT('Origin',(1.23743686707646,-1.23743686707646,2.9));
#9564=CARTESIAN_POINT('',(1.07243686707646,-1.23743686707646,2.9));
#9565=CARTESIAN_POINT('Origin',(1.23743686707646,-1.23743686707646,2.9));
#9566=CARTESIAN_POINT('',(1.07243686707646,-1.23743686707646,3.6));
#9567=CARTESIAN_POINT('',(1.07243686707646,-1.23743686707646,2.9));
#9568=CARTESIAN_POINT('Origin',(1.23743686707646,-1.23743686707646,3.6));
#9569=CARTESIAN_POINT('Origin',(1.23743686707646,-1.23743686707646,2.9));
#9570=CARTESIAN_POINT('Origin',(-1.76776695296637,-1.76776695296637,2.4));
#9571=CARTESIAN_POINT('',(-1.8139637388702,-1.24480341984751,2.4));
#9572=CARTESIAN_POINT('',(-1.24480341984751,-1.81396373887019,2.4));
#9573=CARTESIAN_POINT('Origin',(0.,0.,2.4));
#9574=CARTESIAN_POINT('Origin',(-1.76776695296637,-1.76776695296637,2.4));
#9575=CARTESIAN_POINT('Origin',(-1.76776695296637,-1.76776695296637,1.8));
#9576=CARTESIAN_POINT('',(-1.8139637388702,-1.24480341984751,1.8));
#9577=CARTESIAN_POINT('',(-1.8139637388702,-1.24480341984751,1.8));
#9578=CARTESIAN_POINT('',(-1.24480341984751,-1.81396373887019,1.8));
#9579=CARTESIAN_POINT('Origin',(-1.76776695296637,-1.76776695296637,1.8));
#9580=CARTESIAN_POINT('',(-1.24480341984751,-1.81396373887019,1.8));
#9581=CARTESIAN_POINT('Origin',(-1.76776695296637,1.76776695296637,1.8));
#9582=CARTESIAN_POINT('',(-1.81396373887019,1.24480341984751,2.4));
#9583=CARTESIAN_POINT('',(-1.81396373887019,1.24480341984751,1.8));
#9584=CARTESIAN_POINT('',(-1.81396373887019,1.24480341984751,1.8));
#9585=CARTESIAN_POINT('',(-1.24480341984751,1.81396373887019,2.4));
#9586=CARTESIAN_POINT('Origin',(-1.76776695296637,1.76776695296637,2.4));
#9587=CARTESIAN_POINT('',(-1.24480341984751,1.81396373887019,1.8));
#9588=CARTESIAN_POINT('',(-1.24480341984751,1.81396373887019,1.8));
#9589=CARTESIAN_POINT('Origin',(-1.76776695296637,1.76776695296637,1.8));
#9590=CARTESIAN_POINT('Origin',(-1.76776695296637,1.76776695296637,2.4));
#9591=CARTESIAN_POINT('Origin',(0.,0.,2.4));
#9592=CARTESIAN_POINT('Origin',(1.76776695296637,1.76776695296637,1.8));
#9593=CARTESIAN_POINT('',(1.24480341984751,1.81396373887019,2.4));
#9594=CARTESIAN_POINT('',(1.24480341984751,1.81396373887019,1.8));
#9595=CARTESIAN_POINT('',(1.24480341984751,1.81396373887019,1.8));
#9596=CARTESIAN_POINT('',(1.81396373887019,1.24480341984751,2.4));
#9597=CARTESIAN_POINT('Origin',(1.76776695296637,1.76776695296637,2.4));
#9598=CARTESIAN_POINT('',(1.81396373887019,1.24480341984751,1.8));
#9599=CARTESIAN_POINT('',(1.81396373887019,1.24480341984751,1.8));
#9600=CARTESIAN_POINT('Origin',(1.76776695296637,1.76776695296637,1.8));
#9601=CARTESIAN_POINT('Origin',(1.76776695296637,1.76776695296637,2.4));
#9602=CARTESIAN_POINT('Origin',(0.,0.,2.4));
#9603=CARTESIAN_POINT('Origin',(1.76776695296637,-1.76776695296637,1.8));
#9604=CARTESIAN_POINT('',(1.81396373887019,-1.24480341984751,2.4));
#9605=CARTESIAN_POINT('',(1.81396373887019,-1.24480341984751,1.8));
#9606=CARTESIAN_POINT('',(1.81396373887019,-1.24480341984751,1.8));
#9607=CARTESIAN_POINT('',(1.24480341984751,-1.8139637388702,2.4));
#9608=CARTESIAN_POINT('Origin',(1.76776695296637,-1.76776695296637,2.4));
#9609=CARTESIAN_POINT('',(1.24480341984751,-1.8139637388702,1.8));
#9610=CARTESIAN_POINT('',(1.24480341984751,-1.8139637388702,1.8));
#9611=CARTESIAN_POINT('Origin',(1.76776695296637,-1.76776695296637,1.8));
#9612=CARTESIAN_POINT('Origin',(1.76776695296637,-1.76776695296637,2.4));
#9613=CARTESIAN_POINT('Origin',(0.,0.,2.4));
#9614=CARTESIAN_POINT('Origin',(0.,0.,1.));
#9615=CARTESIAN_POINT('',(-2.2,-2.69422295812418E-16,3.6));
#9616=CARTESIAN_POINT('Origin',(0.,0.,3.6));
#9617=CARTESIAN_POINT('',(-2.2,-2.69422295812418E-16,1.8));
#9618=CARTESIAN_POINT('',(-2.2,-2.69422295812418E-16,1.));
#9619=CARTESIAN_POINT('Origin',(0.,0.,1.8));
#9620=CARTESIAN_POINT('Origin',(0.,0.,1.8));
#9621=CARTESIAN_POINT('Origin',(0.,0.,1.8));
#9622=CARTESIAN_POINT('Origin',(0.,0.,1.8));
#9623=CARTESIAN_POINT('Origin',(0.,0.,1.8));
#9624=CARTESIAN_POINT('Origin',(0.,0.,1.8));
#9625=CARTESIAN_POINT('',(-3.,-3.67394039744206E-16,1.8));
#9626=CARTESIAN_POINT('Origin',(0.,0.,1.8));
#9627=CARTESIAN_POINT('',(-2.04276695296637,-1.76776695296637,1.8));
#9628=CARTESIAN_POINT('Origin',(-1.76776695296637,-1.76776695296637,1.8));
#9629=CARTESIAN_POINT('',(1.49276695296637,1.76776695296637,1.8));
#9630=CARTESIAN_POINT('Origin',(1.76776695296637,1.76776695296637,1.8));
#9631=CARTESIAN_POINT('',(1.49276695296637,-1.76776695296637,1.8));
#9632=CARTESIAN_POINT('Origin',(1.76776695296637,-1.76776695296637,1.8));
#9633=CARTESIAN_POINT('',(-2.04276695296637,1.76776695296637,1.8));
#9634=CARTESIAN_POINT('Origin',(-1.76776695296637,1.76776695296637,1.8));
#9635=CARTESIAN_POINT('Origin',(-1.76776695296637,-1.76776695296637,0.9));
#9636=CARTESIAN_POINT('',(-2.04276695296637,-1.76776695296637,1.));
#9637=CARTESIAN_POINT('Origin',(-1.76776695296637,-1.76776695296637,1.));
#9638=CARTESIAN_POINT('',(-2.04276695296637,-1.76776695296637,0.9));
#9639=CARTESIAN_POINT('Origin',(-1.76776695296637,1.76776695296637,0.9));
#9640=CARTESIAN_POINT('',(-2.04276695296637,1.76776695296637,1.));
#9641=CARTESIAN_POINT('Origin',(-1.76776695296637,1.76776695296637,1.));
#9642=CARTESIAN_POINT('',(-2.04276695296637,1.76776695296637,0.9));
#9643=CARTESIAN_POINT('Origin',(1.76776695296637,1.76776695296637,0.9));
#9644=CARTESIAN_POINT('',(1.49276695296637,1.76776695296637,1.));
#9645=CARTESIAN_POINT('Origin',(1.76776695296637,1.76776695296637,1.));
#9646=CARTESIAN_POINT('',(1.49276695296637,1.76776695296637,0.9));
#9647=CARTESIAN_POINT('Origin',(1.76776695296637,-1.76776695296637,0.9));
#9648=CARTESIAN_POINT('',(1.49276695296637,-1.76776695296637,1.));
#9649=CARTESIAN_POINT('Origin',(1.76776695296637,-1.76776695296637,1.));
#9650=CARTESIAN_POINT('',(1.49276695296637,-1.76776695296637,0.9));
#9651=CARTESIAN_POINT('Origin',(0.,0.,2.05));
#9652=CARTESIAN_POINT('',(-1.5,-1.83697019872103E-16,2.05));
#9653=CARTESIAN_POINT('Origin',(0.,0.,2.05));
#9654=CARTESIAN_POINT('',(-1.5,1.83697019872103E-16,3.6));
#9655=CARTESIAN_POINT('',(-1.5,-1.83697019872103E-16,2.05));
#9656=CARTESIAN_POINT('Origin',(0.,0.,3.6));
#9657=CARTESIAN_POINT('Origin',(0.,0.,2.05));
#9658=CARTESIAN_POINT('',(-1.02,-1.2491397351303E-16,2.05));
#9659=CARTESIAN_POINT('Origin',(0.,0.,2.05));
#9660=CARTESIAN_POINT('Origin',(0.,0.,1.));
#9661=CARTESIAN_POINT('',(-3.,-3.67394039744206E-16,1.));
#9662=CARTESIAN_POINT('',(-3.,-3.67394039744206E-16,1.));
#9663=CARTESIAN_POINT('Origin',(0.,0.,1.));
#9664=CARTESIAN_POINT('Origin',(0.,0.,1.));
#9665=CARTESIAN_POINT('',(-1.02,-1.2491397351303E-16,1.));
#9666=CARTESIAN_POINT('',(-1.02,-1.2491397351303E-16,1.));
#9667=CARTESIAN_POINT('Origin',(0.,0.,1.));
#9668=CARTESIAN_POINT('Origin',(0.,0.,3.6));
#9669=CARTESIAN_POINT('Origin',(0.,0.,1.));
#9670=CARTESIAN_POINT('',(0.,0.,0.));
#9671=CARTESIAN_POINT('Origin',(-1.23743686707646,-1.23743686707646,4.));
#9672=CARTESIAN_POINT('',(-1.61243686707646,-1.23743686707646,4.));
#9673=CARTESIAN_POINT('Origin',(-1.23743686707646,-1.23743686707646,4.));
#9674=CARTESIAN_POINT('',(-1.61243686707646,-1.23743686707646,4.4));
#9675=CARTESIAN_POINT('',(-1.61243686707646,-1.23743686707646,4.));
#9676=CARTESIAN_POINT('Origin',(-1.23743686707646,-1.23743686707646,4.4));
#9677=CARTESIAN_POINT('Origin',(-1.23743686707646,-1.23743686707646,4.));
#9678=CARTESIAN_POINT('',(-1.46243686707646,-1.23743686707646,4.));
#9679=CARTESIAN_POINT('Origin',(-1.23743686707646,-1.23743686707646,4.));
#9680=CARTESIAN_POINT('Origin',(-1.23743686707646,1.23743686707646,4.));
#9681=CARTESIAN_POINT('',(-1.61243686707646,1.23743686707646,4.));
#9682=CARTESIAN_POINT('Origin',(-1.23743686707646,1.23743686707646,4.));
#9683=CARTESIAN_POINT('',(-1.61243686707646,1.23743686707646,4.4));
#9684=CARTESIAN_POINT('',(-1.61243686707646,1.23743686707646,4.));
#9685=CARTESIAN_POINT('Origin',(-1.23743686707646,1.23743686707646,4.4));
#9686=CARTESIAN_POINT('Origin',(-1.23743686707646,1.23743686707646,4.));
#9687=CARTESIAN_POINT('',(-1.46243686707646,1.23743686707646,4.));
#9688=CARTESIAN_POINT('Origin',(-1.23743686707646,1.23743686707646,4.));
#9689=CARTESIAN_POINT('Origin',(1.23743686707646,1.23743686707646,4.));
#9690=CARTESIAN_POINT('',(0.862436867076458,1.23743686707646,4.));
#9691=CARTESIAN_POINT('Origin',(1.23743686707646,1.23743686707646,4.));
#9692=CARTESIAN_POINT('',(0.862436867076458,1.23743686707646,4.4));
#9693=CARTESIAN_POINT('',(0.862436867076458,1.23743686707646,4.));
#9694=CARTESIAN_POINT('Origin',(1.23743686707646,1.23743686707646,4.4));
#9695=CARTESIAN_POINT('Origin',(1.23743686707646,1.23743686707646,4.));
#9696=CARTESIAN_POINT('',(1.01243686707646,1.23743686707646,4.));
#9697=CARTESIAN_POINT('Origin',(1.23743686707646,1.23743686707646,4.));
#9698=CARTESIAN_POINT('Origin',(1.23743686707646,-1.23743686707646,4.));
#9699=CARTESIAN_POINT('',(0.862436867076458,-1.23743686707646,4.));
#9700=CARTESIAN_POINT('Origin',(1.23743686707646,-1.23743686707646,4.));
#9701=CARTESIAN_POINT('',(0.862436867076458,-1.23743686707646,4.4));
#9702=CARTESIAN_POINT('',(0.862436867076458,-1.23743686707646,4.));
#9703=CARTESIAN_POINT('Origin',(1.23743686707646,-1.23743686707646,4.4));
#9704=CARTESIAN_POINT('Origin',(1.23743686707646,-1.23743686707646,4.));
#9705=CARTESIAN_POINT('',(1.01243686707646,-1.23743686707646,4.));
#9706=CARTESIAN_POINT('Origin',(1.23743686707646,-1.23743686707646,4.));
#9707=CARTESIAN_POINT('Origin',(-1.23743686707646,-1.23743686707646,3.5));
#9708=CARTESIAN_POINT('',(-1.46243686707646,-1.23743686707646,3.6));
#9709=CARTESIAN_POINT('Origin',(-1.23743686707646,-1.23743686707646,3.6));
#9710=CARTESIAN_POINT('',(-1.46243686707646,-1.23743686707646,3.5));
#9711=CARTESIAN_POINT('Origin',(-1.23743686707646,1.23743686707646,3.5));
#9712=CARTESIAN_POINT('',(-1.46243686707646,1.23743686707646,3.6));
#9713=CARTESIAN_POINT('Origin',(-1.23743686707646,1.23743686707646,3.6));
#9714=CARTESIAN_POINT('',(-1.46243686707646,1.23743686707646,3.5));
#9715=CARTESIAN_POINT('Origin',(1.23743686707646,1.23743686707646,3.5));
#9716=CARTESIAN_POINT('',(1.01243686707646,1.23743686707646,3.6));
#9717=CARTESIAN_POINT('Origin',(1.23743686707646,1.23743686707646,3.6));
#9718=CARTESIAN_POINT('',(1.01243686707646,1.23743686707646,3.5));
#9719=CARTESIAN_POINT('Origin',(1.23743686707646,-1.23743686707646,3.5));
#9720=CARTESIAN_POINT('',(1.01243686707646,-1.23743686707646,3.6));
#9721=CARTESIAN_POINT('Origin',(1.23743686707646,-1.23743686707646,3.6));
#9722=CARTESIAN_POINT('',(1.01243686707646,-1.23743686707646,3.5));
#9723=CARTESIAN_POINT('Origin',(0.,0.,2.95));
#9724=CARTESIAN_POINT('',(-1.49,-1.82472373072956E-16,3.6));
#9725=CARTESIAN_POINT('Origin',(0.,0.,3.6));
#9726=CARTESIAN_POINT('',(-1.49,-1.82472373072956E-16,2.95));
#9727=CARTESIAN_POINT('',(-1.49,-1.82472373072956E-16,2.95));
#9728=CARTESIAN_POINT('Origin',(0.,0.,2.95));
#9729=CARTESIAN_POINT('Origin',(0.,0.,2.95));
#9730=CARTESIAN_POINT('',(-0.71,-8.69499227394621E-17,2.95));
#9731=CARTESIAN_POINT('Origin',(0.,0.,2.95));
#9732=CARTESIAN_POINT('Origin',(0.,0.,3.6));
#9733=CARTESIAN_POINT('',(-0.71,-8.69499227394621E-17,4.4));
#9734=CARTESIAN_POINT('Origin',(0.,0.,4.4));
#9735=CARTESIAN_POINT('',(-0.71,-8.69499227394621E-17,3.6));
#9736=CARTESIAN_POINT('Origin',(0.,0.,3.6));
#9737=CARTESIAN_POINT('',(-2.2,-2.69422295812418E-16,4.4));
#9738=CARTESIAN_POINT('Origin',(0.,0.,4.4));
#9739=CARTESIAN_POINT('',(-2.2,-2.69422295812418E-16,3.6));
#9740=CARTESIAN_POINT('',(-2.2,-2.69422295812418E-16,3.6));
#9741=CARTESIAN_POINT('Origin',(0.,0.,3.6));
#9742=CARTESIAN_POINT('Origin',(0.,0.,4.4));
#9743=CARTESIAN_POINT('Origin',(0.,0.,3.6));
#9744=CARTESIAN_POINT('',(0.,0.,0.));
#9745=CARTESIAN_POINT('',(0.,0.,0.));
#9746=CARTESIAN_POINT('Origin',(0.75,1.2,0.));
#9747=CARTESIAN_POINT('',(0.885663593019381,1.2,-0.16));
#9748=CARTESIAN_POINT('',(0.885663593019381,1.2,0.16));
#9749=CARTESIAN_POINT('Origin',(0.,1.2,0.));
#9750=CARTESIAN_POINT('',(0.93,1.2,-0.16));
#9751=CARTESIAN_POINT('',(0.93,1.2,-0.16));
#9752=CARTESIAN_POINT('',(0.93,1.2,0.16));
#9753=CARTESIAN_POINT('',(0.93,1.2,0.16));
#9754=CARTESIAN_POINT('',(0.57,1.2,0.16));
#9755=CARTESIAN_POINT('Origin',(0.57,0.,0.16));
#9756=CARTESIAN_POINT('',(0.885663593019381,-1.2,0.16));
#9757=CARTESIAN_POINT('',(0.885663593019381,0.,0.16));
#9758=CARTESIAN_POINT('',(0.93,-1.2,0.16));
#9759=CARTESIAN_POINT('',(0.93,0.,0.16));
#9760=CARTESIAN_POINT('',(0.57,-1.2,0.16));
#9761=CARTESIAN_POINT('Origin',(0.75,-1.2,0.));
#9762=CARTESIAN_POINT('',(0.885663593019381,-1.2,-0.16));
#9763=CARTESIAN_POINT('Origin',(0.,-1.2,0.));
#9764=CARTESIAN_POINT('',(0.93,-1.2,-0.16));
#9765=CARTESIAN_POINT('',(0.93,-1.2,0.16));
#9766=CARTESIAN_POINT('',(0.93,-1.2,-0.16));
#9767=CARTESIAN_POINT('Origin',(0.93,0.,-0.16));
#9768=CARTESIAN_POINT('',(0.885663593019381,0.,-0.16));
#9769=CARTESIAN_POINT('',(0.93,0.,-0.16));
#9770=CARTESIAN_POINT('Origin',(0.93,0.,0.16));
#9771=CARTESIAN_POINT('Origin',(1.05,1.5,0.));
#9772=CARTESIAN_POINT('',(-1.05,1.5,-1.28587913910472E-16));
#9773=CARTESIAN_POINT('Origin',(0.,1.5,0.));
#9774=CARTESIAN_POINT('',(-0.9,1.5,-1.10218211923262E-16));
#9775=CARTESIAN_POINT('Origin',(0.,1.5,0.));
#9776=CARTESIAN_POINT('Origin',(0.,1.315,0.));
#9777=CARTESIAN_POINT('',(-1.05,1.13,-1.28587913910472E-16));
#9778=CARTESIAN_POINT('Origin',(0.,1.13,0.));
#9779=CARTESIAN_POINT('',(-1.05,1.315,-1.28587913910472E-16));
#9780=CARTESIAN_POINT('Origin',(1.,1.13,0.));
#9781=CARTESIAN_POINT('',(-1.,1.13,-1.22464679914735E-16));
#9782=CARTESIAN_POINT('Origin',(0.,1.13,0.));
#9783=CARTESIAN_POINT('Origin',(0.,1.065,0.));
#9784=CARTESIAN_POINT('',(-1.,1.,-1.22464679914735E-16));
#9785=CARTESIAN_POINT('Origin',(0.,1.,0.));
#9786=CARTESIAN_POINT('',(-1.,1.065,-1.22464679914735E-16));
#9787=CARTESIAN_POINT('Origin',(1.05,1.,0.));
#9788=CARTESIAN_POINT('',(-1.05,1.,-1.28587913910472E-16));
#9789=CARTESIAN_POINT('Origin',(0.,1.,0.));
#9790=CARTESIAN_POINT('Origin',(0.,0.,0.));
#9791=CARTESIAN_POINT('',(-1.05,-1.,-1.28587913910472E-16));
#9792=CARTESIAN_POINT('Origin',(0.,-1.,0.));
#9793=CARTESIAN_POINT('',(-1.05,0.,-1.28587913910472E-16));
#9794=CARTESIAN_POINT('Origin',(1.,-1.,0.));
#9795=CARTESIAN_POINT('',(-1.,-1.,-1.22464679914735E-16));
#9796=CARTESIAN_POINT('Origin',(0.,-1.,0.));
#9797=CARTESIAN_POINT('Origin',(0.,-1.065,0.));
#9798=CARTESIAN_POINT('',(-1.,-1.13,-1.22464679914735E-16));
#9799=CARTESIAN_POINT('Origin',(0.,-1.13,0.));
#9800=CARTESIAN_POINT('',(-1.,-1.065,-1.22464679914735E-16));
#9801=CARTESIAN_POINT('Origin',(1.05,-1.13,0.));
#9802=CARTESIAN_POINT('',(-1.05,-1.13,-1.28587913910472E-16));
#9803=CARTESIAN_POINT('Origin',(0.,-1.13,0.));
#9804=CARTESIAN_POINT('Origin',(0.,-1.315,0.));
#9805=CARTESIAN_POINT('',(-1.05,-1.5,-1.28587913910472E-16));
#9806=CARTESIAN_POINT('Origin',(0.,-1.5,0.));
#9807=CARTESIAN_POINT('',(-1.05,-1.315,-1.28587913910472E-16));
#9808=CARTESIAN_POINT('Origin',(0.9,-1.5,0.));
#9809=CARTESIAN_POINT('',(-0.9,-1.5,-1.10218211923262E-16));
#9810=CARTESIAN_POINT('Origin',(0.,-1.5,0.));
#9811=CARTESIAN_POINT('Origin',(0.,0.,0.));
#9812=CARTESIAN_POINT('',(-0.9,0.,-1.10218211923262E-16));
#9813=CARTESIAN_POINT('',(0.,0.,0.));
#9814=CARTESIAN_POINT('Origin',(0.75,1.2,0.));
#9815=CARTESIAN_POINT('',(0.880582193778639,1.2,0.16));
#9816=CARTESIAN_POINT('',(0.880582193778639,1.2,-0.16));
#9817=CARTESIAN_POINT('Origin',(0.,1.2,0.));
#9818=CARTESIAN_POINT('',(0.583459510163302,1.2,0.16));
#9819=CARTESIAN_POINT('',(0.57,1.2,0.16));
#9820=CARTESIAN_POINT('',(0.583459510163302,1.2,-0.16));
#9821=CARTESIAN_POINT('Origin',(0.,1.2,0.));
#9822=CARTESIAN_POINT('',(0.93,1.2,-0.16));
#9823=CARTESIAN_POINT('Origin',(0.93,0.,-0.16));
#9824=CARTESIAN_POINT('',(0.880582193778639,-1.2,-0.16));
#9825=CARTESIAN_POINT('',(0.880582193778639,0.,-0.16));
#9826=CARTESIAN_POINT('',(0.583459510163302,-1.2,-0.16));
#9827=CARTESIAN_POINT('',(0.583459510163302,0.,-0.16));
#9828=CARTESIAN_POINT('',(0.93,-1.2,-0.16));
#9829=CARTESIAN_POINT('Origin',(0.75,-1.2,0.));
#9830=CARTESIAN_POINT('',(0.880582193778639,-1.2,0.16));
#9831=CARTESIAN_POINT('Origin',(0.,-1.2,0.));
#9832=CARTESIAN_POINT('',(0.583459510163302,-1.2,0.16));
#9833=CARTESIAN_POINT('Origin',(0.,-1.2,0.));
#9834=CARTESIAN_POINT('',(0.57,-1.2,0.16));
#9835=CARTESIAN_POINT('Origin',(0.57,0.,0.16));
#9836=CARTESIAN_POINT('',(0.880582193778639,0.,0.16));
#9837=CARTESIAN_POINT('',(0.583459510163302,0.,0.16));
#9838=CARTESIAN_POINT('Origin',(0.895,1.35,0.));
#9839=CARTESIAN_POINT('',(-0.895,1.35,-1.09605888523688E-16));
#9840=CARTESIAN_POINT('Origin',(0.,1.35,0.));
#9841=CARTESIAN_POINT('',(-0.605,1.35,-7.40911313484149E-17));
#9842=CARTESIAN_POINT('Origin',(0.,1.35,0.));
#9843=CARTESIAN_POINT('Origin',(0.,0.,0.));
#9844=CARTESIAN_POINT('',(-0.895,-1.35,-1.09605888523688E-16));
#9845=CARTESIAN_POINT('Origin',(0.,-1.35,0.));
#9846=CARTESIAN_POINT('',(-0.895,0.,-1.09605888523688E-16));
#9847=CARTESIAN_POINT('Origin',(0.605,-1.35,0.));
#9848=CARTESIAN_POINT('',(-0.605,-1.35,-7.40911313484149E-17));
#9849=CARTESIAN_POINT('Origin',(0.,-1.35,0.));
#9850=CARTESIAN_POINT('Origin',(0.,0.,0.));
#9851=CARTESIAN_POINT('',(-0.605,0.,-7.40911313484149E-17));
#9852=CARTESIAN_POINT('',(0.,0.,0.));
#9853=CARTESIAN_POINT('',(0.,0.,0.));
#9854=CARTESIAN_POINT('',(0.,0.,0.));
#9855=CARTESIAN_POINT('Origin',(0.115470053837925,-0.5,-0.2));
#9856=CARTESIAN_POINT('',(0.23094010767585,-0.5,0.));
#9857=CARTESIAN_POINT('',(0.115470053837925,-0.5,-0.2));
#9858=CARTESIAN_POINT('',(0.23094010767585,-0.5,0.));
#9859=CARTESIAN_POINT('',(0.115470053837925,-0.8,-0.2));
#9860=CARTESIAN_POINT('',(0.115470053837925,-0.5,-0.2));
#9861=CARTESIAN_POINT('',(0.23094010767585,-0.8,0.));
#9862=CARTESIAN_POINT('',(0.23094010767585,-0.8,0.));
#9863=CARTESIAN_POINT('',(0.23094010767585,-0.5,0.));
#9864=CARTESIAN_POINT('Origin',(-0.115470053837925,-0.5,-0.2));
#9865=CARTESIAN_POINT('',(-0.115470053837925,-0.5,-0.2));
#9866=CARTESIAN_POINT('',(0.115470053837925,-0.5,-0.2));
#9867=CARTESIAN_POINT('',(-0.115470053837925,-0.8,-0.2));
#9868=CARTESIAN_POINT('',(-0.115470053837925,-0.5,-0.2));
#9869=CARTESIAN_POINT('',(0.115470053837925,-0.8,-0.2));
#9870=CARTESIAN_POINT('Origin',(-0.23094010767585,-0.5,-2.77555756156289E-17));
#9871=CARTESIAN_POINT('',(-0.23094010767585,-0.5,-2.82820063659975E-17));
#9872=CARTESIAN_POINT('',(-0.115470053837925,-0.5,-0.2));
#9873=CARTESIAN_POINT('',(-0.23094010767585,-0.8,-2.77555756156289E-17));
#9874=CARTESIAN_POINT('',(-0.23094010767585,-0.5,-2.82820063659975E-17));
#9875=CARTESIAN_POINT('',(-0.115470053837925,-0.8,-0.2));
#9876=CARTESIAN_POINT('Origin',(-0.115470053837925,-0.5,0.2));
#9877=CARTESIAN_POINT('',(-0.115470053837925,-0.5,0.2));
#9878=CARTESIAN_POINT('',(-0.23094010767585,-0.5,-2.82820063659975E-17));
#9879=CARTESIAN_POINT('',(-0.115470053837925,-0.8,0.2));
#9880=CARTESIAN_POINT('',(-0.115470053837925,-0.5,0.2));
#9881=CARTESIAN_POINT('',(-0.23094010767585,-0.8,-2.82820063659975E-17));
#9882=CARTESIAN_POINT('Origin',(0.115470053837925,-0.5,0.2));
#9883=CARTESIAN_POINT('',(0.115470053837925,-0.5,0.2));
#9884=CARTESIAN_POINT('',(-0.115470053837925,-0.5,0.2));
#9885=CARTESIAN_POINT('',(0.115470053837925,-0.8,0.2));
#9886=CARTESIAN_POINT('',(0.115470053837925,-0.5,0.2));
#9887=CARTESIAN_POINT('',(-0.115470053837925,-0.8,0.2));
#9888=CARTESIAN_POINT('Origin',(0.23094010767585,-0.5,0.));
#9889=CARTESIAN_POINT('',(0.115470053837925,-0.5,0.2));
#9890=CARTESIAN_POINT('',(0.115470053837925,-0.8,0.2));
#9891=CARTESIAN_POINT('Origin',(0.,-0.5,0.));
#9892=CARTESIAN_POINT('Origin',(0.,-0.8,0.));
#9893=CARTESIAN_POINT('Origin',(0.,-1.4,0.));
#9894=CARTESIAN_POINT('',(-0.24505,-1.4,3.00099698131059E-17));
#9895=CARTESIAN_POINT('Origin',(0.,-1.4,0.));
#9896=CARTESIAN_POINT('Origin',(0.375,0.5,0.));
#9897=CARTESIAN_POINT('',(-0.375,0.5,-4.59242549680257E-17));
#9898=CARTESIAN_POINT('Origin',(0.,0.5,0.));
#9899=CARTESIAN_POINT('Origin',(0.,0.475,0.));
#9900=CARTESIAN_POINT('',(-0.425,0.45,-5.20474889637625E-17));
#9901=CARTESIAN_POINT('Origin',(0.,0.45,0.));
#9902=CARTESIAN_POINT('',(-0.4,0.475,-4.89858719658941E-17));
#9903=CARTESIAN_POINT('Origin',(0.,0.24,0.));
#9904=CARTESIAN_POINT('',(-0.425,0.0299999999999998,-5.20474889637625E-17));
#9905=CARTESIAN_POINT('Origin',(0.,0.0299999999999998,0.));
#9906=CARTESIAN_POINT('',(-0.425,0.24,-5.20474889637625E-17));
#9907=CARTESIAN_POINT('Origin',(0.,0.0150000000000001,0.));
#9908=CARTESIAN_POINT('',(-0.395,4.85722573273506E-17,-4.83735485663204E-17));
#9909=CARTESIAN_POINT('Origin',(0.,0.,0.));
#9910=CARTESIAN_POINT('',(-0.41,0.0150000000000001,-5.02105187650415E-17));
#9911=CARTESIAN_POINT('Origin',(0.27,0.,0.));
#9912=CARTESIAN_POINT('',(-0.27,0.,-3.30654635769785E-17));
#9913=CARTESIAN_POINT('Origin',(0.,0.,0.));
#9914=CARTESIAN_POINT('Origin',(0.,-0.02,0.));
#9915=CARTESIAN_POINT('',(-0.24505,-0.0498999999999999,3.00099698131059E-17));
#9916=CARTESIAN_POINT('Origin',(0.,-0.0498999999999999,0.));
#9917=CARTESIAN_POINT('',(-0.26,-0.02,-3.18408167778312E-17));
#9918=CARTESIAN_POINT('Origin',(0.,-0.995,0.));
#9919=CARTESIAN_POINT('',(-0.24505,-0.995,-3.00099698131059E-17));
#9920=CARTESIAN_POINT('',(0.,0.,0.));
#9921=CARTESIAN_POINT('',(0.,0.,0.));
#9922=CARTESIAN_POINT('Origin',(0.5,0.,5.7));
#9923=CARTESIAN_POINT('',(-2.49742622740447,-3.67078843507121E-16,5.7));
#9924=CARTESIAN_POINT('Origin',(0.5,0.,5.7));
#9925=CARTESIAN_POINT('',(-0.5,-6.12323399573677E-17,5.7));
#9926=CARTESIAN_POINT('Origin',(0.,0.,5.7));
#9927=CARTESIAN_POINT('Origin',(0.5,0.,4.8));
#9928=CARTESIAN_POINT('',(-2.49742622740447,-3.67078843507121E-16,4.8));
#9929=CARTESIAN_POINT('Origin',(0.5,0.,4.8));
#9930=CARTESIAN_POINT('',(-0.7,-8.57252759403147E-17,4.8));
#9931=CARTESIAN_POINT('Origin',(0.,0.,4.8));
#9932=CARTESIAN_POINT('Origin',(0.5,0.,4.8));
#9933=CARTESIAN_POINT('',(-2.49742622740447,-3.67078843507121E-16,4.8));
#9934=CARTESIAN_POINT('Origin',(0.,0.,2.95));
#9935=CARTESIAN_POINT('',(-0.7,-8.57252759403147E-17,2.95));
#9936=CARTESIAN_POINT('Origin',(0.,0.,2.95));
#9937=CARTESIAN_POINT('',(-0.5,6.12323399573677E-17,2.95));
#9938=CARTESIAN_POINT('Origin',(0.,0.,2.95));
#9939=CARTESIAN_POINT('Origin',(0.,0.,2.95));
#9940=CARTESIAN_POINT('',(-0.7,-8.57252759403147E-17,2.95));
#9941=CARTESIAN_POINT('Origin',(0.,0.,1.));
#9942=CARTESIAN_POINT('',(-0.5,-6.12323399573677E-17,1.));
#9943=CARTESIAN_POINT('',(-0.5,-6.12323399573677E-17,1.));
#9944=CARTESIAN_POINT('Origin',(0.,0.,1.));
#9945=CARTESIAN_POINT('Origin',(0.,0.,1.));
#9946=CARTESIAN_POINT('',(-0.5,-6.12323399573677E-17,6.));
#9947=CARTESIAN_POINT('Origin',(0.,0.,6.));
#9948=CARTESIAN_POINT('',(-0.5,-6.12323399573677E-17,1.));
#9949=CARTESIAN_POINT('Origin',(0.,0.,6.));
#9950=CARTESIAN_POINT('Origin',(0.,0.,1.));
#9951=CARTESIAN_POINT('',(0.,0.,0.));
#9952=CARTESIAN_POINT('Origin',(0.,0.,1.8));
#9953=CARTESIAN_POINT('',(-0.505,-6.18446633569413E-17,2.05));
#9954=CARTESIAN_POINT('Origin',(0.,0.,2.05));
#9955=CARTESIAN_POINT('',(-0.505,-6.18446633569413E-17,1.8));
#9956=CARTESIAN_POINT('',(-0.505,-6.18446633569413E-17,1.8));
#9957=CARTESIAN_POINT('Origin',(0.,0.,1.8));
#9958=CARTESIAN_POINT('Origin',(0.,0.,1.8));
#9959=CARTESIAN_POINT('',(-0.7,-8.57252759403147E-17,2.05));
#9960=CARTESIAN_POINT('Origin',(0.,0.,2.05));
#9961=CARTESIAN_POINT('',(-0.7,-8.57252759403147E-17,1.8));
#9962=CARTESIAN_POINT('',(-0.7,-8.57252759403147E-17,1.8));
#9963=CARTESIAN_POINT('Origin',(0.,0.,1.8));
#9964=CARTESIAN_POINT('Origin',(0.,0.,2.05));
#9965=CARTESIAN_POINT('Origin',(0.,0.,1.8));
#9966=CARTESIAN_POINT('',(0.,0.,0.));
#9967=CARTESIAN_POINT('Origin',(0.49,0.,1.4));
#9968=CARTESIAN_POINT('',(0.49,0.122167917228706,1.28909463493591));
#9969=CARTESIAN_POINT('',(0.49,0.122167917228706,1.51090536506409));
#9970=CARTESIAN_POINT('',(0.49,0.122167917228706,1.));
#9971=CARTESIAN_POINT('Origin',(0.49,0.,1.4));
#9972=CARTESIAN_POINT('Origin',(0.49,0.,1.4));
#9973=CARTESIAN_POINT('',(0.49,-0.122167917228706,1.28909463493591));
#9974=CARTESIAN_POINT('Ctrl Pts',(0.49,-0.122167917228706,1.28909463493591));
#9975=CARTESIAN_POINT('Ctrl Pts',(0.490448531679987,-0.120368913626296,
1.28711294069536));
#9976=CARTESIAN_POINT('Ctrl Pts',(0.490895245371685,-0.118534896565231,
1.28518965877367));
#9977=CARTESIAN_POINT('Ctrl Pts',(0.494795015531646,-0.102111993019358,
1.2687667552278));
#9978=CARTESIAN_POINT('Ctrl Pts',(0.498442514607594,-0.0836597150224318,
1.25609154388858));
#9979=CARTESIAN_POINT('Ctrl Pts',(0.50357781976106,-0.0430495960471595,
1.23920409039234));
#9980=CARTESIAN_POINT('Ctrl Pts',(0.505,-0.020880094330741,1.235));
#9981=CARTESIAN_POINT('Ctrl Pts',(0.505,0.020880094330741,1.235));
#9982=CARTESIAN_POINT('Ctrl Pts',(0.50357781976106,0.0430495960471595,1.23920409039234));
#9983=CARTESIAN_POINT('Ctrl Pts',(0.498442514607594,0.0836597150224318,
1.25609154388858));
#9984=CARTESIAN_POINT('Ctrl Pts',(0.494795015531646,0.102111993019358,1.2687667552278));
#9985=CARTESIAN_POINT('Ctrl Pts',(0.490895245371684,0.118534896565231,1.28518965877367));
#9986=CARTESIAN_POINT('Ctrl Pts',(0.490448531679987,0.120368913626296,1.28711294069536));
#9987=CARTESIAN_POINT('Ctrl Pts',(0.49,0.122167917228706,1.28909463493591));
#9988=CARTESIAN_POINT('',(0.49,-0.122167917228706,1.51090536506409));
#9989=CARTESIAN_POINT('Origin',(0.49,0.,1.4));
#9990=CARTESIAN_POINT('',(0.505,-1.70422299968729E-17,1.565));
#9991=CARTESIAN_POINT('Ctrl Pts',(0.505,-6.93889390390723E-18,1.565));
#9992=CARTESIAN_POINT('Ctrl Pts',(0.505,-0.020880094330741,1.565));
#9993=CARTESIAN_POINT('Ctrl Pts',(0.50357781976106,-0.0430495960471595,
1.56079590960766));
#9994=CARTESIAN_POINT('Ctrl Pts',(0.498442514607594,-0.0836597150224318,
1.54390845611142));
#9995=CARTESIAN_POINT('Ctrl Pts',(0.494795015531646,-0.102111993019358,
1.5312332447722));
#9996=CARTESIAN_POINT('Ctrl Pts',(0.490895245371684,-0.118534896565231,
1.51481034122633));
#9997=CARTESIAN_POINT('Ctrl Pts',(0.490448531679987,-0.120368913626296,
1.51288705930464));
#9998=CARTESIAN_POINT('Ctrl Pts',(0.49,-0.122167917228706,1.51090536506409));
#9999=CARTESIAN_POINT('',(0.9,-2.02066721859313E-17,1.565));
#10000=CARTESIAN_POINT('',(0.49,-2.02066721859313E-17,1.565));
#10001=CARTESIAN_POINT('',(0.884745726183518,0.165,1.4));
#10002=CARTESIAN_POINT('Ctrl Pts',(0.884745726183518,0.165,1.4));
#10003=CARTESIAN_POINT('Ctrl Pts',(0.884745726183518,0.165,1.37923124059256));
#10004=CARTESIAN_POINT('Ctrl Pts',(0.885552759505264,0.160839719007584,
1.35711110492666));
#10005=CARTESIAN_POINT('Ctrl Pts',(0.888448648150043,0.143986470216691,
1.31647293736623));
#10006=CARTESIAN_POINT('Ctrl Pts',(0.890493604851638,0.131295993814186,
1.29795075602263));
#10007=CARTESIAN_POINT('Ctrl Pts',(0.89431723432394,0.102049819008125,1.26870458121656));
#10008=CARTESIAN_POINT('Ctrl Pts',(0.896347088899543,0.0835273920906824,
1.25601365401642));
#10009=CARTESIAN_POINT('Ctrl Pts',(0.899208271860583,0.0428883760934127,
1.23916007816136));
#10010=CARTESIAN_POINT('Ctrl Pts',(0.9,0.0207679427235068,1.235));
#10011=CARTESIAN_POINT('Ctrl Pts',(0.9,-0.0207679427235068,1.235));
#10012=CARTESIAN_POINT('Ctrl Pts',(0.899208271860583,-0.0428883760934127,
1.23916007816136));
#10013=CARTESIAN_POINT('Ctrl Pts',(0.896347088899543,-0.0835273920906823,
1.25601365401642));
#10014=CARTESIAN_POINT('Ctrl Pts',(0.89431723432394,-0.102049819008125,
1.26870458121656));
#10015=CARTESIAN_POINT('Ctrl Pts',(0.890493604851638,-0.131295993814186,
1.29795075602263));
#10016=CARTESIAN_POINT('Ctrl Pts',(0.888448648150043,-0.143986470216691,
1.31647293736623));
#10017=CARTESIAN_POINT('Ctrl Pts',(0.885552759505264,-0.160839719007584,
1.35711110492666));
#10018=CARTESIAN_POINT('Ctrl Pts',(0.884745726183518,-0.165,1.37923124059256));
#10019=CARTESIAN_POINT('Ctrl Pts',(0.884745726183518,-0.165,1.42076875940744));
#10020=CARTESIAN_POINT('Ctrl Pts',(0.885552759505264,-0.160839719007584,
1.44288889507334));
#10021=CARTESIAN_POINT('Ctrl Pts',(0.888448648150043,-0.14398647021669,
1.48352706263377));
#10022=CARTESIAN_POINT('Ctrl Pts',(0.890493604851638,-0.131295993814186,
1.50204924397737));
#10023=CARTESIAN_POINT('Ctrl Pts',(0.89431723432394,-0.102049819008125,
1.53129541878344));
#10024=CARTESIAN_POINT('Ctrl Pts',(0.896347088899543,-0.0835273920906824,
1.54398634598358));
#10025=CARTESIAN_POINT('Ctrl Pts',(0.899208271860583,-0.0428883760934128,
1.56083992183864));
#10026=CARTESIAN_POINT('Ctrl Pts',(0.9,-0.0207679427235068,1.565));
#10027=CARTESIAN_POINT('Ctrl Pts',(0.9,-6.93889390390723E-18,1.565));
#10028=CARTESIAN_POINT('Ctrl Pts',(0.9,-3.46944695195361E-17,1.565));
#10029=CARTESIAN_POINT('Ctrl Pts',(0.9,0.0207679427235068,1.565));
#10030=CARTESIAN_POINT('Ctrl Pts',(0.899208271860583,0.0428883760934127,
1.56083992183864));
#10031=CARTESIAN_POINT('Ctrl Pts',(0.896347088899543,0.0835273920906824,
1.54398634598358));
#10032=CARTESIAN_POINT('Ctrl Pts',(0.89431723432394,0.102049819008125,1.53129541878344));
#10033=CARTESIAN_POINT('Ctrl Pts',(0.890493604851638,0.131295993814186,
1.50204924397737));
#10034=CARTESIAN_POINT('Ctrl Pts',(0.888448648150043,0.143986470216691,
1.48352706263377));
#10035=CARTESIAN_POINT('Ctrl Pts',(0.885552759505264,0.160839719007584,
1.44288889507334));
#10036=CARTESIAN_POINT('Ctrl Pts',(0.884745726183518,0.165,1.42076875940744));
#10037=CARTESIAN_POINT('Ctrl Pts',(0.884745726183518,0.165,1.4));
#10038=CARTESIAN_POINT('Ctrl Pts',(0.49,0.122167917228706,1.51090536506409));
#10039=CARTESIAN_POINT('Ctrl Pts',(0.490448531679987,0.120368913626296,
1.51288705930464));
#10040=CARTESIAN_POINT('Ctrl Pts',(0.490895245371685,0.118534896565231,
1.51481034122633));
#10041=CARTESIAN_POINT('Ctrl Pts',(0.494795015531646,0.102111993019358,
1.5312332447722));
#10042=CARTESIAN_POINT('Ctrl Pts',(0.498442514607594,0.0836597150224318,
1.54390845611142));
#10043=CARTESIAN_POINT('Ctrl Pts',(0.50357781976106,0.0430495960471594,
1.56079590960766));
#10044=CARTESIAN_POINT('Ctrl Pts',(0.505,0.020880094330741,1.565));
#10045=CARTESIAN_POINT('Ctrl Pts',(0.505,0.,1.565));
#10046=CARTESIAN_POINT('Origin',(0.49,0.,1.4));
#10047=CARTESIAN_POINT('',(0.49,-0.122167917228706,1.));
#10048=CARTESIAN_POINT('Origin',(0.,0.,1.));
#10049=CARTESIAN_POINT('',(-0.505,-6.18446633569413E-17,1.8));
#10050=CARTESIAN_POINT('Origin',(0.,0.,1.8));
#10051=CARTESIAN_POINT('',(-0.505,-6.18446633569413E-17,1.));
#10052=CARTESIAN_POINT('',(-0.505,-6.18446633569413E-17,1.));
#10053=CARTESIAN_POINT('Origin',(0.,0.,1.));
#10054=CARTESIAN_POINT('Origin',(0.,0.,1.));
#10055=CARTESIAN_POINT('',(-0.9,-1.10218211923262E-16,1.8));
#10056=CARTESIAN_POINT('Origin',(0.,0.,1.8));
#10057=CARTESIAN_POINT('',(-0.9,-1.10218211923262E-16,1.));
#10058=CARTESIAN_POINT('',(-0.9,-1.10218211923262E-16,1.));
#10059=CARTESIAN_POINT('Origin',(0.,0.,1.));
#10060=CARTESIAN_POINT('Origin',(0.,0.,1.8));
#10061=CARTESIAN_POINT('Origin',(0.,0.,1.));
#10062=CARTESIAN_POINT('',(0.,0.,0.));
#10063=CARTESIAN_POINT('Origin',(0.,-0.4,0.));
#10064=CARTESIAN_POINT('',(-0.1954,-0.4,2.39295984553393E-17));
#10065=CARTESIAN_POINT('Origin',(0.,-0.4,0.));
#10066=CARTESIAN_POINT('Origin',(0.0577350269189626,0.,-0.1));
#10067=CARTESIAN_POINT('',(0.0577350269189626,0.,-0.1));
#10068=CARTESIAN_POINT('',(0.115470053837925,0.,0.));
#10069=CARTESIAN_POINT('',(0.0934187836487032,0.,-0.0381939203391614));
#10070=CARTESIAN_POINT('',(0.0577350269189626,-0.2,-0.1));
#10071=CARTESIAN_POINT('',(0.0577350269189626,0.,-0.1));
#10072=CARTESIAN_POINT('',(0.115470053837925,-0.2,0.));
#10073=CARTESIAN_POINT('',(0.115470053837925,-0.2,0.));
#10074=CARTESIAN_POINT('',(0.115470053837925,0.,0.));
#10075=CARTESIAN_POINT('Origin',(-0.0577350269189626,0.,-0.1));
#10076=CARTESIAN_POINT('',(-0.0577350269189626,0.,-0.1));
#10077=CARTESIAN_POINT('',(0.0561324865405187,0.,-0.1));
#10078=CARTESIAN_POINT('',(-0.0577350269189626,-0.2,-0.1));
#10079=CARTESIAN_POINT('',(-0.0577350269189626,0.,-0.1));
#10080=CARTESIAN_POINT('',(0.0577350269189626,-0.2,-0.1));
#10081=CARTESIAN_POINT('Origin',(-0.115470053837925,0.,-1.38777878078145E-17));
#10082=CARTESIAN_POINT('',(-0.115470053837925,0.,-1.41410031829988E-17));
#10083=CARTESIAN_POINT('',(-0.0797862971081845,0.,-0.0618060796608387));
#10084=CARTESIAN_POINT('',(-0.115470053837925,-0.2,-1.38777878078145E-17));
#10085=CARTESIAN_POINT('',(-0.115470053837925,0.,-1.41410031829988E-17));
#10086=CARTESIAN_POINT('',(-0.0577350269189626,-0.2,-0.1));
#10087=CARTESIAN_POINT('Origin',(-0.0577350269189626,0.,0.1));
#10088=CARTESIAN_POINT('',(-0.0577350269189626,0.,0.1));
#10089=CARTESIAN_POINT('',(-0.0509187836487033,0.,0.111806079660839));
#10090=CARTESIAN_POINT('',(-0.0577350269189626,-0.2,0.1));
#10091=CARTESIAN_POINT('',(-0.0577350269189626,0.,0.1));
#10092=CARTESIAN_POINT('',(-0.115470053837925,-0.2,-1.41410031829988E-17));
#10093=CARTESIAN_POINT('Origin',(0.0577350269189626,0.,0.1));
#10094=CARTESIAN_POINT('',(0.0577350269189626,0.,0.1));
#10095=CARTESIAN_POINT('',(0.113867513459481,0.,0.1));
#10096=CARTESIAN_POINT('',(0.0577350269189626,-0.2,0.1));
#10097=CARTESIAN_POINT('',(0.0577350269189626,0.,0.1));
#10098=CARTESIAN_POINT('',(-0.0577350269189626,-0.2,0.1));
#10099=CARTESIAN_POINT('Origin',(0.115470053837925,0.,0.));
#10100=CARTESIAN_POINT('',(0.122286297108185,0.,-0.0118060796608386));
#10101=CARTESIAN_POINT('',(0.0577350269189626,-0.2,0.1));
#10102=CARTESIAN_POINT('Origin',(0.,-0.2,0.));
#10103=CARTESIAN_POINT('Origin',(0.17,0.,0.));
#10104=CARTESIAN_POINT('',(-0.17,-8.67361737988404E-18,-2.0818995585505E-17));
#10105=CARTESIAN_POINT('Origin',(0.,0.,0.));
#10106=CARTESIAN_POINT('Origin',(0.,-0.015,0.));
#10107=CARTESIAN_POINT('',(-0.1954,-0.0254,-2.39295984553393E-17));
#10108=CARTESIAN_POINT('Origin',(0.,-0.0254,0.));
#10109=CARTESIAN_POINT('',(-0.185,-0.015,-2.2655965784226E-17));
#10110=CARTESIAN_POINT('Origin',(0.,-0.2775,0.));
#10111=CARTESIAN_POINT('',(-0.1954,-0.2775,-2.39295984553393E-17));
#10112=CARTESIAN_POINT('',(0.,0.,0.));
#10113=CARTESIAN_POINT('',(0.,0.,0.));
#10114=CARTESIAN_POINT('',(0.,0.,0.));
#10115=CARTESIAN_POINT('',(0.9,0.,1.4));
#10116=CARTESIAN_POINT('',(0.,0.,0.));
#10117=CARTESIAN_POINT('',(0.,0.,0.));
#10118=CARTESIAN_POINT('Origin',(6.2,0.,5.25));
#10119=CARTESIAN_POINT('',(6.2,-0.6,4.45));
#10120=CARTESIAN_POINT('',(6.2,-0.6,6.05));
#10121=CARTESIAN_POINT('',(6.2,-0.6,5.775));
#10122=CARTESIAN_POINT('Origin',(6.2,0.,5.25));
#10123=CARTESIAN_POINT('Origin',(6.2,0.,5.25));
#10124=CARTESIAN_POINT('',(6.2,0.6,6.05));
#10125=CARTESIAN_POINT('',(6.2,0.6,4.45));
#10126=CARTESIAN_POINT('',(6.2,0.6,4.725));
#10127=CARTESIAN_POINT('Origin',(6.2,0.,5.25));
#10128=CARTESIAN_POINT('Origin',(6.2,0.,5.25));
#10129=CARTESIAN_POINT('',(6.4,-0.6,4.45));
#10130=CARTESIAN_POINT('',(6.2,-0.6,4.45));
#10131=CARTESIAN_POINT('',(6.4,-0.6,6.05));
#10132=CARTESIAN_POINT('Origin',(6.4,0.,5.25));
#10133=CARTESIAN_POINT('',(6.2,-0.6,6.05));
#10134=CARTESIAN_POINT('Origin',(6.2,0.,5.25));
#10135=CARTESIAN_POINT('',(6.4,0.6,4.45));
#10136=CARTESIAN_POINT('',(6.2,0.6,4.45));
#10137=CARTESIAN_POINT('',(6.4,0.6,6.05));
#10138=CARTESIAN_POINT('',(6.2,0.6,6.05));
#10139=CARTESIAN_POINT('Origin',(6.4,0.,5.25));
#10140=CARTESIAN_POINT('Origin',(6.4,0.,5.25));
#10141=CARTESIAN_POINT('',(6.4,0.6,6.3));
#10142=CARTESIAN_POINT('',(6.4,0.6,4.2));
#10143=CARTESIAN_POINT('',(6.4,-0.6,6.3));
#10144=CARTESIAN_POINT('',(6.4,0.6,6.3));
#10145=CARTESIAN_POINT('',(6.4,-0.6,6.3));
#10146=CARTESIAN_POINT('',(6.4,-0.6,4.2));
#10147=CARTESIAN_POINT('',(6.4,-0.6,6.3));
#10148=CARTESIAN_POINT('',(6.4,0.6,4.2));
#10149=CARTESIAN_POINT('',(6.4,-0.6,4.2));
#10150=CARTESIAN_POINT('',(6.4,0.6,4.2));
#10151=CARTESIAN_POINT('',(6.4,-7.34788079488412E-17,5.85));
#10152=CARTESIAN_POINT('Origin',(6.4,0.,5.25));
#10153=CARTESIAN_POINT('Origin',(5.8,-0.6,6.3));
#10154=CARTESIAN_POINT('',(4.,-0.6,6.3));
#10155=CARTESIAN_POINT('',(4.,-0.6,6.3));
#10156=CARTESIAN_POINT('',(4.,-0.6,5.9));
#10157=CARTESIAN_POINT('',(4.,-0.6,5.9));
#10158=CARTESIAN_POINT('',(5.8,-0.6,5.9));
#10159=CARTESIAN_POINT('',(4.,-0.6,5.9));
#10160=CARTESIAN_POINT('',(5.8,-0.6,4.6));
#10161=CARTESIAN_POINT('',(5.8,-0.6,6.3));
#10162=CARTESIAN_POINT('',(4.,-0.6,4.6));
#10163=CARTESIAN_POINT('',(4.,-0.6,4.6));
#10164=CARTESIAN_POINT('',(4.,-0.6,4.2));
#10165=CARTESIAN_POINT('',(4.,-0.6,4.2));
#10166=CARTESIAN_POINT('',(5.8,-0.6,4.2));
#10167=CARTESIAN_POINT('Origin',(4.,0.,4.1));
#10168=CARTESIAN_POINT('',(3.49,-6.2456986756515E-17,4.2));
#10169=CARTESIAN_POINT('Origin',(4.,0.,4.2));
#10170=CARTESIAN_POINT('',(3.49,6.2456986756515E-17,4.6));
#10171=CARTESIAN_POINT('',(3.49,-6.2456986756515E-17,4.1));
#10172=CARTESIAN_POINT('Origin',(4.,0.,4.6));
#10173=CARTESIAN_POINT('Origin',(4.,0.,4.1));
#10174=CARTESIAN_POINT('',(3.49,-6.2456986756515E-17,5.9));
#10175=CARTESIAN_POINT('Origin',(4.,0.,5.9));
#10176=CARTESIAN_POINT('',(3.49,6.2456986756515E-17,6.3));
#10177=CARTESIAN_POINT('',(3.49,-6.2456986756515E-17,4.1));
#10178=CARTESIAN_POINT('Origin',(4.,0.,6.3));
#10179=CARTESIAN_POINT('Origin',(4.,0.,5.9));
#10180=CARTESIAN_POINT('',(4.,0.6,5.9));
#10181=CARTESIAN_POINT('',(4.,0.6,6.3));
#10182=CARTESIAN_POINT('',(4.,0.6,5.9));
#10183=CARTESIAN_POINT('Origin',(4.,0.,5.9));
#10184=CARTESIAN_POINT('Origin',(4.,0.,6.3));
#10185=CARTESIAN_POINT('Origin',(5.8,0.6,6.3));
#10186=CARTESIAN_POINT('',(5.8,0.6,6.3));
#10187=CARTESIAN_POINT('Origin',(5.05,0.,5.9));
#10188=CARTESIAN_POINT('',(5.8,0.6,5.9));
#10189=CARTESIAN_POINT('',(6.1,0.6,5.9));
#10190=CARTESIAN_POINT('',(5.8,0.,5.9));
#10191=CARTESIAN_POINT('Origin',(5.8,0.6,4.2));
#10192=CARTESIAN_POINT('',(4.,0.6,4.2));
#10193=CARTESIAN_POINT('',(5.8,0.6,4.2));
#10194=CARTESIAN_POINT('',(4.,0.6,4.6));
#10195=CARTESIAN_POINT('',(4.,0.6,4.2));
#10196=CARTESIAN_POINT('',(5.8,0.6,4.6));
#10197=CARTESIAN_POINT('',(6.1,0.6,4.6));
#10198=CARTESIAN_POINT('',(5.8,0.6,4.2));
#10199=CARTESIAN_POINT('Origin',(4.,0.,4.2));
#10200=CARTESIAN_POINT('Origin',(4.,0.,4.6));
#10201=CARTESIAN_POINT('Origin',(4.,0.,4.2));
#10202=CARTESIAN_POINT('Origin',(5.8,-0.6,4.2));
#10203=CARTESIAN_POINT('Origin',(5.05,0.,4.6));
#10204=CARTESIAN_POINT('',(5.8,0.,4.6));
#10205=CARTESIAN_POINT('Origin',(5.8,0.,5.25));
#10206=CARTESIAN_POINT('',(14.,-7.34788079488412E-17,5.85));
#10207=CARTESIAN_POINT('Origin',(14.,0.,5.25));
#10208=CARTESIAN_POINT('',(5.8,-7.34788079488412E-17,5.85));
#10209=CARTESIAN_POINT('Origin',(14.,0.,5.25));
#10210=CARTESIAN_POINT('Origin',(5.8,0.,5.25));
#10211=CARTESIAN_POINT('',(0.,0.,0.));
#10212=CARTESIAN_POINT('Origin',(4.,0.,5.2));
#10213=CARTESIAN_POINT('',(3.835,-2.02066721859313E-17,5.2));
#10214=CARTESIAN_POINT('Origin',(4.,0.,5.2));
#10215=CARTESIAN_POINT('',(3.835,2.02066721859313E-17,6.3));
#10216=CARTESIAN_POINT('',(3.835,-2.02066721859313E-17,5.2));
#10217=CARTESIAN_POINT('Origin',(4.,0.,6.3));
#10218=CARTESIAN_POINT('Origin',(4.,0.,5.2));
#10219=CARTESIAN_POINT('Origin',(4.,0.,4.2));
#10220=CARTESIAN_POINT('',(3.3,-8.57252759403147E-17,4.2));
#10221=CARTESIAN_POINT('Origin',(4.,0.,4.2));
#10222=CARTESIAN_POINT('',(3.5,-6.12323399573677E-17,4.2));
#10223=CARTESIAN_POINT('Origin',(4.,0.,4.2));
#10224=CARTESIAN_POINT('Origin',(4.,0.,4.));
#10225=CARTESIAN_POINT('',(3.3,-8.57252759403147E-17,4.));
#10226=CARTESIAN_POINT('',(3.3,-8.57252759403147E-17,4.));
#10227=CARTESIAN_POINT('Origin',(4.,0.,4.));
#10228=CARTESIAN_POINT('Origin',(4.,0.,4.));
#10229=CARTESIAN_POINT('Origin',(4.,0.,4.2));
#10230=CARTESIAN_POINT('',(3.5,-6.12323399573677E-17,6.3));
#10231=CARTESIAN_POINT('Origin',(4.,0.,6.3));
#10232=CARTESIAN_POINT('',(3.5,-6.12323399573677E-17,4.2));
#10233=CARTESIAN_POINT('Origin',(4.,0.,6.3));
#10234=CARTESIAN_POINT('',(0.,0.,0.));
#10235=CARTESIAN_POINT('Origin',(4.,0.,4.6));
#10236=CARTESIAN_POINT('',(3.495,-6.18446633569413E-17,4.8));
#10237=CARTESIAN_POINT('Origin',(4.,0.,4.8));
#10238=CARTESIAN_POINT('',(3.495,-6.18446633569413E-17,4.6));
#10239=CARTESIAN_POINT('',(3.495,-6.18446633569413E-17,4.6));
#10240=CARTESIAN_POINT('Origin',(4.,0.,4.6));
#10241=CARTESIAN_POINT('Origin',(4.,0.,4.6));
#10242=CARTESIAN_POINT('',(3.3,-8.57252759403147E-17,4.8));
#10243=CARTESIAN_POINT('Origin',(4.,0.,4.8));
#10244=CARTESIAN_POINT('',(3.3,-8.57252759403147E-17,4.6));
#10245=CARTESIAN_POINT('',(3.3,-8.57252759403147E-17,4.6));
#10246=CARTESIAN_POINT('Origin',(4.,0.,4.6));
#10247=CARTESIAN_POINT('Origin',(4.,0.,4.8));
#10248=CARTESIAN_POINT('Origin',(4.,0.,4.6));
#10249=CARTESIAN_POINT('',(0.,0.,0.));
#10250=CARTESIAN_POINT('Origin',(4.,0.,5.7));
#10251=CARTESIAN_POINT('',(3.495,-6.18446633569413E-17,5.9));
#10252=CARTESIAN_POINT('Origin',(4.,0.,5.9));
#10253=CARTESIAN_POINT('',(3.495,-6.18446633569413E-17,5.7));
#10254=CARTESIAN_POINT('',(3.495,-6.18446633569413E-17,5.7));
#10255=CARTESIAN_POINT('Origin',(4.,0.,5.7));
#10256=CARTESIAN_POINT('Origin',(4.,0.,5.7));
#10257=CARTESIAN_POINT('',(3.3,-8.57252759403147E-17,5.9));
#10258=CARTESIAN_POINT('Origin',(4.,0.,5.9));
#10259=CARTESIAN_POINT('',(3.3,-8.57252759403147E-17,5.7));
#10260=CARTESIAN_POINT('',(3.3,-8.57252759403147E-17,5.7));
#10261=CARTESIAN_POINT('Origin',(4.,0.,5.7));
#10262=CARTESIAN_POINT('Origin',(4.,0.,5.9));
#10263=CARTESIAN_POINT('Origin',(4.,0.,5.7));
#10264=CARTESIAN_POINT('',(0.,0.,0.));
#10265=CARTESIAN_POINT('Origin',(4.,0.,6.3));
#10266=CARTESIAN_POINT('',(3.775,-2.75545529808154E-17,6.5));
#10267=CARTESIAN_POINT('Origin',(4.,0.,6.5));
#10268=CARTESIAN_POINT('',(3.775,-2.75545529808154E-17,6.3));
#10269=CARTESIAN_POINT('',(3.775,-2.75545529808154E-17,6.3));
#10270=CARTESIAN_POINT('Origin',(4.,0.,6.3));
#10271=CARTESIAN_POINT('Origin',(4.,0.,6.3));
#10272=CARTESIAN_POINT('',(3.3,-8.57252759403147E-17,6.5));
#10273=CARTESIAN_POINT('Origin',(4.,0.,6.5));
#10274=CARTESIAN_POINT('',(3.3,-8.57252759403147E-17,6.3));
#10275=CARTESIAN_POINT('',(3.3,-8.57252759403147E-17,6.3));
#10276=CARTESIAN_POINT('Origin',(4.,0.,6.3));
#10277=CARTESIAN_POINT('Origin',(4.,0.,6.5));
#10278=CARTESIAN_POINT('Origin',(4.,0.,6.3));
#10279=CARTESIAN_POINT('',(0.,0.,0.));
#10280=CARTESIAN_POINT('Origin',(0.0866025403784439,-0.4,-0.15));
#10281=CARTESIAN_POINT('',(0.173205080756888,-0.4,0.));
#10282=CARTESIAN_POINT('',(0.0866025403784439,-0.4,-0.15));
#10283=CARTESIAN_POINT('',(0.173205080756888,-0.4,0.));
#10284=CARTESIAN_POINT('',(0.0866025403784439,-0.64,-0.15));
#10285=CARTESIAN_POINT('',(0.0866025403784439,-0.4,-0.15));
#10286=CARTESIAN_POINT('',(0.173205080756888,-0.64,0.));
#10287=CARTESIAN_POINT('',(0.173205080756888,-0.64,0.));
#10288=CARTESIAN_POINT('',(0.173205080756888,-0.4,0.));
#10289=CARTESIAN_POINT('Origin',(-0.0866025403784438,-0.4,-0.15));
#10290=CARTESIAN_POINT('',(-0.0866025403784438,-0.4,-0.15));
#10291=CARTESIAN_POINT('',(0.0866025403784439,-0.4,-0.15));
#10292=CARTESIAN_POINT('',(-0.0866025403784438,-0.64,-0.15));
#10293=CARTESIAN_POINT('',(-0.0866025403784438,-0.4,-0.15));
#10294=CARTESIAN_POINT('',(0.0866025403784439,-0.64,-0.15));
#10295=CARTESIAN_POINT('Origin',(-0.173205080756888,-0.4,-2.77555756156289E-17));
#10296=CARTESIAN_POINT('',(-0.173205080756888,-0.4,-2.12115047744981E-17));
#10297=CARTESIAN_POINT('',(-0.0866025403784438,-0.4,-0.15));
#10298=CARTESIAN_POINT('',(-0.173205080756888,-0.64,-2.77555756156289E-17));
#10299=CARTESIAN_POINT('',(-0.173205080756888,-0.4,-2.12115047744981E-17));
#10300=CARTESIAN_POINT('',(-0.0866025403784438,-0.64,-0.15));
#10301=CARTESIAN_POINT('Origin',(-0.0866025403784439,-0.4,0.15));
#10302=CARTESIAN_POINT('',(-0.0866025403784439,-0.4,0.15));
#10303=CARTESIAN_POINT('',(-0.173205080756888,-0.4,-2.12115047744981E-17));
#10304=CARTESIAN_POINT('',(-0.0866025403784439,-0.64,0.15));
#10305=CARTESIAN_POINT('',(-0.0866025403784439,-0.4,0.15));
#10306=CARTESIAN_POINT('',(-0.173205080756888,-0.64,-2.12115047744981E-17));
#10307=CARTESIAN_POINT('Origin',(0.0866025403784439,-0.4,0.15));
#10308=CARTESIAN_POINT('',(0.0866025403784439,-0.4,0.15));
#10309=CARTESIAN_POINT('',(-0.0866025403784439,-0.4,0.15));
#10310=CARTESIAN_POINT('',(0.0866025403784439,-0.64,0.15));
#10311=CARTESIAN_POINT('',(0.0866025403784439,-0.4,0.15));
#10312=CARTESIAN_POINT('',(-0.0866025403784439,-0.64,0.15));
#10313=CARTESIAN_POINT('Origin',(0.173205080756888,-0.4,0.));
#10314=CARTESIAN_POINT('',(0.0866025403784439,-0.4,0.15));
#10315=CARTESIAN_POINT('',(0.0866025403784439,-0.64,0.15));
#10316=CARTESIAN_POINT('Origin',(0.,-0.4,-2.77555756156289E-17));
#10317=CARTESIAN_POINT('Origin',(0.,-0.64,-2.77555756156289E-17));
#10318=CARTESIAN_POINT('Origin',(0.,-1.,0.));
#10319=CARTESIAN_POINT('',(-0.1954,-1.,2.39295984553393E-17));
#10320=CARTESIAN_POINT('Origin',(0.,-1.,0.));
#10321=CARTESIAN_POINT('Origin',(0.3,0.4,0.));
#10322=CARTESIAN_POINT('',(-0.3,0.4,-3.67394039744206E-17));
#10323=CARTESIAN_POINT('Origin',(0.,0.4,0.));
#10324=CARTESIAN_POINT('Origin',(0.,0.375,0.));
#10325=CARTESIAN_POINT('',(-0.35,0.35,-4.28626379701573E-17));
#10326=CARTESIAN_POINT('Origin',(0.,0.35,0.));
#10327=CARTESIAN_POINT('',(-0.325,0.375,-3.9801020972289E-17));
#10328=CARTESIAN_POINT('Origin',(0.,0.19,0.));
#10329=CARTESIAN_POINT('',(-0.35,0.03,-4.28626379701574E-17));
#10330=CARTESIAN_POINT('Origin',(0.,0.03,0.));
#10331=CARTESIAN_POINT('',(-0.35,0.19,-4.28626379701574E-17));
#10332=CARTESIAN_POINT('Origin',(0.,0.0149999999999999,0.));
#10333=CARTESIAN_POINT('',(-0.32,-3.29597460435593E-17,-3.91886975727153E-17));
#10334=CARTESIAN_POINT('Origin',(0.,0.,0.));
#10335=CARTESIAN_POINT('',(-0.335,0.0149999999999999,-4.10256677714363E-17));
#10336=CARTESIAN_POINT('Origin',(0.22,0.,0.));
#10337=CARTESIAN_POINT('',(-0.22,-6.93889390390723E-18,-2.69422295812418E-17));
#10338=CARTESIAN_POINT('Origin',(0.,0.,0.));
#10339=CARTESIAN_POINT('Origin',(0.,-0.02,0.));
#10340=CARTESIAN_POINT('',(-0.1954,-0.0492,2.39295984553393E-17));
#10341=CARTESIAN_POINT('Origin',(0.,-0.0492,0.));
#10342=CARTESIAN_POINT('',(-0.21,-0.02,-2.57175827820944E-17));
#10343=CARTESIAN_POINT('Origin',(0.,-0.8,0.));
#10344=CARTESIAN_POINT('',(-0.1954,-0.8,-2.39295984553393E-17));
#10345=CARTESIAN_POINT('',(0.,0.,0.));
#10346=CARTESIAN_POINT('',(0.,0.,0.));
#10347=CARTESIAN_POINT('',(0.,0.,0.));
#10348=CARTESIAN_POINT('',(0.,0.,0.));
#10349=CARTESIAN_POINT('',(0.,0.,0.));
#10350=CARTESIAN_POINT('',(4.,0.,6.5));
#10351=CARTESIAN_POINT('',(0.,0.,0.));
#10352=CARTESIAN_POINT('',(0.,0.,0.));
#10353=CARTESIAN_POINT('',(0.,0.,0.));
#10354=CARTESIAN_POINT('Origin',(0.,0.,0.));
#10355=CARTESIAN_POINT('',(-0.976185,-0.246528389340863,-1.19548183562566E-16));
#10356=CARTESIAN_POINT('',(-1.19548183562566E-16,-0.246528389340863,0.976185));
#10357=CARTESIAN_POINT('Origin',(0.,-0.246528389340863,0.));
#10358=CARTESIAN_POINT('Origin',(0.,-0.246528389340863,0.));
#10359=CARTESIAN_POINT('',(-1.19548183562566E-16,0.246528389340863,0.976185));
#10360=CARTESIAN_POINT('Origin',(-1.22464679914735E-16,0.,1.));
#10361=CARTESIAN_POINT('',(-0.976185,0.246528389340863,1.19548183562566E-16));
#10362=CARTESIAN_POINT('Origin',(0.,0.246528389340863,0.));
#10363=CARTESIAN_POINT('Origin',(0.,0.246528389340863,0.));
#10364=CARTESIAN_POINT('Origin',(0.,0.,0.));
#10365=CARTESIAN_POINT('',(-0.976185,0.45,-1.19548183562566E-16));
#10366=CARTESIAN_POINT('',(-0.976185,0.,-1.19548183562566E-16));
#10367=CARTESIAN_POINT('Origin',(0.,0.45,0.));
#10368=CARTESIAN_POINT('Origin',(0.,0.,0.));
#10369=CARTESIAN_POINT('',(-0.5,-0.39,-6.12323399573677E-17));
#10370=CARTESIAN_POINT('Origin',(0.,-0.39,0.));
#10371=CARTESIAN_POINT('',(-0.5,0.39,-6.12323399573677E-17));
#10372=CARTESIAN_POINT('',(-0.5,0.,-6.12323399573677E-17));
#10373=CARTESIAN_POINT('Origin',(0.,0.39,0.));
#10374=CARTESIAN_POINT('Origin',(0.,0.42,0.));
#10375=CARTESIAN_POINT('',(-0.56,0.45,-6.85802207522518E-17));
#10376=CARTESIAN_POINT('',(-0.53,0.42,-6.49062803548097E-17));
#10377=CARTESIAN_POINT('Origin',(0.,0.45,0.));
#10378=CARTESIAN_POINT('Origin',(0.976185,0.45,0.));
#10379=CARTESIAN_POINT('Origin',(0.,0.,0.));
#10380=CARTESIAN_POINT('',(-0.976185,-0.45,-1.19548183562566E-16));
#10381=CARTESIAN_POINT('Origin',(0.,-0.45,0.));
#10382=CARTESIAN_POINT('',(-0.976185,0.,-1.19548183562566E-16));
#10383=CARTESIAN_POINT('Origin',(0.56,-0.45,0.));
#10384=CARTESIAN_POINT('',(-0.56,-0.45,-6.85802207522518E-17));
#10385=CARTESIAN_POINT('Origin',(0.,-0.45,0.));
#10386=CARTESIAN_POINT('Origin',(0.,-0.42,0.));
#10387=CARTESIAN_POINT('',(-0.53,-0.42,-6.49062803548097E-17));
#10388=CARTESIAN_POINT('',(0.,0.,0.));
#10389=CARTESIAN_POINT('Origin',(0.,0.,0.));
#10390=CARTESIAN_POINT('',(-1.023815,0.246528389340863,-1.25381176266905E-16));
#10391=CARTESIAN_POINT('',(-1.25381176266905E-16,0.246528389340863,1.023815));
#10392=CARTESIAN_POINT('Origin',(0.,0.246528389340863,0.));
#10393=CARTESIAN_POINT('Origin',(0.,0.246528389340863,0.));
#10394=CARTESIAN_POINT('',(-1.25381176266905E-16,-0.246528389340863,1.023815));
#10395=CARTESIAN_POINT('Origin',(-1.22464679914735E-16,0.,1.));
#10396=CARTESIAN_POINT('',(-1.023815,-0.246528389340863,1.25381176266905E-16));
#10397=CARTESIAN_POINT('Origin',(0.,-0.246528389340863,0.));
#10398=CARTESIAN_POINT('Origin',(0.,-0.246528389340863,0.));
#10399=CARTESIAN_POINT('Origin',(0.,0.,0.));
#10400=CARTESIAN_POINT('',(-1.023815,-0.45,-1.25381176266905E-16));
#10401=CARTESIAN_POINT('Origin',(0.,-0.45,0.));
#10402=CARTESIAN_POINT('',(-1.023815,0.,-1.25381176266905E-16));
#10403=CARTESIAN_POINT('Origin',(1.44,0.45,0.));
#10404=CARTESIAN_POINT('',(-1.44,0.45,-1.76349139077219E-16));
#10405=CARTESIAN_POINT('Origin',(0.,0.45,0.));
#10406=CARTESIAN_POINT('',(-1.023815,0.45,-1.25381176266905E-16));
#10407=CARTESIAN_POINT('Origin',(0.,0.45,0.));
#10408=CARTESIAN_POINT('Origin',(0.,0.42,0.));
#10409=CARTESIAN_POINT('',(-1.5,0.39,-1.83697019872103E-16));
#10410=CARTESIAN_POINT('Origin',(0.,0.39,0.));
#10411=CARTESIAN_POINT('',(-1.47,0.42,-1.80023079474661E-16));
#10412=CARTESIAN_POINT('Origin',(0.,0.,0.));
#10413=CARTESIAN_POINT('',(-1.5,-0.39,-1.83697019872103E-16));
#10414=CARTESIAN_POINT('Origin',(0.,-0.39,0.));
#10415=CARTESIAN_POINT('',(-1.5,0.,-1.83697019872103E-16));
#10416=CARTESIAN_POINT('Origin',(0.,-0.42,0.));
#10417=CARTESIAN_POINT('',(-1.44,-0.45,-1.76349139077219E-16));
#10418=CARTESIAN_POINT('Origin',(0.,-0.45,0.));
#10419=CARTESIAN_POINT('',(-1.47,-0.42,-1.80023079474661E-16));
#10420=CARTESIAN_POINT('Origin',(1.023815,-0.45,0.));
#10421=CARTESIAN_POINT('Origin',(0.,0.,0.));
#10422=CARTESIAN_POINT('',(-1.023815,0.,-1.25381176266905E-16));
#10423=CARTESIAN_POINT('',(0.,0.,0.));
#10424=CARTESIAN_POINT('Origin',(1.,0.,0.));
#10425=CARTESIAN_POINT('',(1.,-1.78583896120461E-33,0.23815));
#10426=CARTESIAN_POINT('',(1.,-1.78583896120461E-33,-0.23815));
#10427=CARTESIAN_POINT('Origin',(1.,0.,0.));
#10428=CARTESIAN_POINT('Origin',(0.707106781186548,0.,-0.707106781186547));
#10429=CARTESIAN_POINT('',(0.875504261126124,-1.78583896120461E-33,-0.538709301246971));
#10430=CARTESIAN_POINT('',(0.538709301246971,-1.78583896120461E-33,-0.875504261126124));
#10431=CARTESIAN_POINT('Origin',(0.707106781186548,0.,-0.707106781186547));
#10432=CARTESIAN_POINT('Origin',(6.12323399573677E-17,0.,-1.));
#10433=CARTESIAN_POINT('',(0.23815,-1.78583896120461E-33,-1.));
#10434=CARTESIAN_POINT('',(-0.23815,-1.78583896120461E-33,-1.));
#10435=CARTESIAN_POINT('Origin',(6.12323399573677E-17,0.,-1.));
#10436=CARTESIAN_POINT('Origin',(-0.707106781186547,0.,-0.707106781186548));
#10437=CARTESIAN_POINT('',(-0.538709301246971,-1.78583896120461E-33,-0.875504261126124));
#10438=CARTESIAN_POINT('',(-0.875504261126124,-1.78583896120461E-33,-0.538709301246971));
#10439=CARTESIAN_POINT('Origin',(-0.707106781186547,0.,-0.707106781186548));
#10440=CARTESIAN_POINT('Origin',(-1.,0.,-1.22464679914735E-16));
#10441=CARTESIAN_POINT('',(-1.,-1.78583896120461E-33,-0.23815));
#10442=CARTESIAN_POINT('',(-1.,-1.78583896120461E-33,0.23815));
#10443=CARTESIAN_POINT('Origin',(-1.,0.,-1.22464679914735E-16));
#10444=CARTESIAN_POINT('Origin',(-0.707106781186548,0.,0.707106781186547));
#10445=CARTESIAN_POINT('',(-0.875504261126124,-7.94881478324376E-33,0.538709301246971));
#10446=CARTESIAN_POINT('',(-0.538709301246971,4.37713686083455E-33,0.875504261126124));
#10447=CARTESIAN_POINT('Origin',(-0.707106781186548,0.,0.707106781186547));
#10448=CARTESIAN_POINT('Origin',(-1.83697019872103E-16,0.,1.));
#10449=CARTESIAN_POINT('',(-0.23815,-1.78583896120461E-33,1.));
#10450=CARTESIAN_POINT('',(0.23815,-1.78583896120461E-33,1.));
#10451=CARTESIAN_POINT('Origin',(-1.83697019872103E-16,0.,1.));
#10452=CARTESIAN_POINT('Origin',(0.707106781186547,0.,0.707106781186548));
#10453=CARTESIAN_POINT('',(0.538709301246971,-4.86732687222419E-33,0.875504261126124));
#10454=CARTESIAN_POINT('',(0.875504261126124,1.29564894981497E-33,0.538709301246971));
#10455=CARTESIAN_POINT('Origin',(0.707106781186547,0.,0.707106781186548));
#10456=CARTESIAN_POINT('',(0.,0.,0.));
#10457=CARTESIAN_POINT('Origin',(0.707106781186547,0.,0.707106781186548));
#10458=CARTESIAN_POINT('',(0.504455939115715,-0.04763,0.841298510752802));
#10459=CARTESIAN_POINT('',(0.841298510752802,-0.04763,0.504455939115715));
#10460=CARTESIAN_POINT('Ctrl Pts',(0.504455939115715,-0.04763,0.841298510752802));
#10461=CARTESIAN_POINT('Ctrl Pts',(0.508899795931835,-0.0740444353928835,
0.838633903678357));
#10462=CARTESIAN_POINT('Ctrl Pts',(0.517157748491652,-0.0999305678883309,
0.833661031856294));
#10463=CARTESIAN_POINT('Ctrl Pts',(0.537715343527944,-0.142345102874864,
0.820511285096538));
#10464=CARTESIAN_POINT('Ctrl Pts',(0.548874290046456,-0.159766064500479,
0.813159949759));
#10465=CARTESIAN_POINT('Ctrl Pts',(0.573915184558107,-0.190326085855194,
0.795684265985089));
#10466=CARTESIAN_POINT('Ctrl Pts',(0.587792702767295,-0.203463743702801,
0.78555112003688));
#10467=CARTESIAN_POINT('Ctrl Pts',(0.615966552324775,-0.224161999508995,
0.763642258217233));
#10468=CARTESIAN_POINT('Ctrl Pts',(0.631684198665438,-0.232861760990032,
0.750785745543687));
#10469=CARTESIAN_POINT('Ctrl Pts',(0.663382628119203,-0.244251601209411,
0.722929908501543));
#10470=CARTESIAN_POINT('Ctrl Pts',(0.679352081686668,-0.246942143572133,
0.707917883896095));
#10471=CARTESIAN_POINT('Ctrl Pts',(0.707917883896095,-0.246942143572133,
0.679352081686668));
#10472=CARTESIAN_POINT('Ctrl Pts',(0.722929908501543,-0.244251601209411,
0.663382628119203));
#10473=CARTESIAN_POINT('Ctrl Pts',(0.750785745543687,-0.232861760990032,
0.631684198665439));
#10474=CARTESIAN_POINT('Ctrl Pts',(0.763642258217232,-0.224161999508995,
0.615966552324775));
#10475=CARTESIAN_POINT('Ctrl Pts',(0.78555112003688,-0.203463743702801,
0.587792702767295));
#10476=CARTESIAN_POINT('Ctrl Pts',(0.795684265985088,-0.190326085855194,
0.573915184558108));
#10477=CARTESIAN_POINT('Ctrl Pts',(0.813159949759,-0.15976606450048,0.548874290046456));
#10478=CARTESIAN_POINT('Ctrl Pts',(0.820511285096538,-0.142345102874864,
0.537715343527944));
#10479=CARTESIAN_POINT('Ctrl Pts',(0.833661031856294,-0.099930567888331,
0.517157748491653));
#10480=CARTESIAN_POINT('Ctrl Pts',(0.838633903678357,-0.0740444353928835,
0.508899795931835));
#10481=CARTESIAN_POINT('Ctrl Pts',(0.841298510752801,-0.0476299999999999,
0.504455939115715));
#10482=CARTESIAN_POINT('',(0.528110872004958,-0.04763,0.871530771444223));
#10483=CARTESIAN_POINT('Origin',(0.707106781186547,-0.04763,0.707106781186548));
#10484=CARTESIAN_POINT('',(0.871530771444223,-0.04763,0.528110872004959));
#10485=CARTESIAN_POINT('Ctrl Pts',(0.871530771444223,-0.0476300000000001,
0.528110872004958));
#10486=CARTESIAN_POINT('Ctrl Pts',(0.87014664509073,-0.0609922781173483,
0.530395067942936));
#10487=CARTESIAN_POINT('Ctrl Pts',(0.868149331745851,-0.0742967091364493,
0.533674141594226));
#10488=CARTESIAN_POINT('Ctrl Pts',(0.85981294420286,-0.115492077056649,
0.54708917182331));
#10489=CARTESIAN_POINT('Ctrl Pts',(0.850993704737257,-0.141695629206859,
0.560922177770136));
#10490=CARTESIAN_POINT('Ctrl Pts',(0.830754510485543,-0.181890537957859,
0.590422647829571));
#10491=CARTESIAN_POINT('Ctrl Pts',(0.816896541396381,-0.201072148666545,
0.609616703125488));
#10492=CARTESIAN_POINT('Ctrl Pts',(0.792310597819928,-0.223955109275652,
0.641117951819998));
#10493=CARTESIAN_POINT('Ctrl Pts',(0.779109323683612,-0.232742381310829,
0.657208095763053));
#10494=CARTESIAN_POINT('Ctrl Pts',(0.750552691816206,-0.244234834628584,
0.68964083160521));
#10495=CARTESIAN_POINT('Ctrl Pts',(0.735185187071673,-0.246942143572133,
0.705971972091755));
#10496=CARTESIAN_POINT('Ctrl Pts',(0.705971972091754,-0.246942143572133,
0.735185187071673));
#10497=CARTESIAN_POINT('Ctrl Pts',(0.689640831605209,-0.244234834628584,
0.750552691816206));
#10498=CARTESIAN_POINT('Ctrl Pts',(0.657208095763052,-0.232742381310829,
0.779109323683612));
#10499=CARTESIAN_POINT('Ctrl Pts',(0.641117951819998,-0.223955109275652,
0.792310597819928));
#10500=CARTESIAN_POINT('Ctrl Pts',(0.609616703125487,-0.201072148666545,
0.816896541396382));
#10501=CARTESIAN_POINT('Ctrl Pts',(0.590422647829571,-0.181890537957858,
0.830754510485544));
#10502=CARTESIAN_POINT('Ctrl Pts',(0.560922177770135,-0.141695629206858,
0.850993704737257));
#10503=CARTESIAN_POINT('Ctrl Pts',(0.547089171823309,-0.115492077056649,
0.859812944202861));
#10504=CARTESIAN_POINT('Ctrl Pts',(0.533674141594226,-0.0742967091364491,
0.868149331745852));
#10505=CARTESIAN_POINT('Ctrl Pts',(0.530395067942936,-0.0609922781173483,
0.870146645090731));
#10506=CARTESIAN_POINT('Ctrl Pts',(0.528110872004958,-0.0476300000000001,
0.871530771444223));
#10507=CARTESIAN_POINT('Origin',(0.707106781186547,-0.04763,0.707106781186548));
#10508=CARTESIAN_POINT('Origin',(0.,-0.166705,0.));
#10509=CARTESIAN_POINT('',(0.242834539687906,-0.04763,0.989696097314));
#10510=CARTESIAN_POINT('Origin',(0.,-0.04763,0.));
#10511=CARTESIAN_POINT('',(-0.242834539687907,-0.04763,0.989696097314));
#10512=CARTESIAN_POINT('Ctrl Pts',(0.242834539687906,-0.04763,0.989696097314));
#10513=CARTESIAN_POINT('Ctrl Pts',(0.24024064412003,-0.0609922781173483,
0.990332542620729));
#10514=CARTESIAN_POINT('Ctrl Pts',(0.236509675094874,-0.0742967091364492,
0.991238884025248));
#10515=CARTESIAN_POINT('Ctrl Pts',(0.221129100087819,-0.115492077056649,
0.994830026707808));
#10516=CARTESIAN_POINT('Ctrl Pts',(0.205111543747588,-0.141695629206859,
0.998375294985966));
#10517=CARTESIAN_POINT('Ctrl Pts',(0.169940289819232,-0.181890537957859,
1.00492400591205));
#10518=CARTESIAN_POINT('Ctrl Pts',(0.1465689792446,-0.201072148666545,1.00869718865384));
#10519=CARTESIAN_POINT('Ctrl Pts',(0.106909345252087,-0.223955109275652,
1.01358704779679));
#10520=CARTESIAN_POINT('Ctrl Pts',(0.0861971848975941,-0.232742381310829,
1.0156297872271));
#10521=CARTESIAN_POINT('Ctrl Pts',(0.0430711894098822,-0.244234834628584,
1.01837060663223));
#10522=CARTESIAN_POINT('Ctrl Pts',(0.0206568624125605,-0.246942143572133,
1.019052));
#10523=CARTESIAN_POINT('Ctrl Pts',(-0.0206568624125608,-0.246942143572133,
1.019052));
#10524=CARTESIAN_POINT('Ctrl Pts',(-0.0430711894098825,-0.244234834628584,
1.01837060663223));
#10525=CARTESIAN_POINT('Ctrl Pts',(-0.0861971848975943,-0.232742381310829,
1.0156297872271));
#10526=CARTESIAN_POINT('Ctrl Pts',(-0.106909345252088,-0.223955109275652,
1.01358704779679));
#10527=CARTESIAN_POINT('Ctrl Pts',(-0.1465689792446,-0.201072148666545,
1.00869718865384));
#10528=CARTESIAN_POINT('Ctrl Pts',(-0.169940289819232,-0.181890537957859,
1.00492400591205));
#10529=CARTESIAN_POINT('Ctrl Pts',(-0.205111543747588,-0.141695629206859,
0.998375294985966));
#10530=CARTESIAN_POINT('Ctrl Pts',(-0.221129100087819,-0.115492077056649,
0.994830026707808));
#10531=CARTESIAN_POINT('Ctrl Pts',(-0.236509675094875,-0.0742967091364493,
0.991238884025248));
#10532=CARTESIAN_POINT('Ctrl Pts',(-0.24024064412003,-0.0609922781173483,
0.990332542620729));
#10533=CARTESIAN_POINT('Ctrl Pts',(-0.242834539687907,-0.04763,0.989696097314));
#10534=CARTESIAN_POINT('',(-0.528110872004959,-0.04763,0.871530771444223));
#10535=CARTESIAN_POINT('Origin',(0.,-0.04763,0.));
#10536=CARTESIAN_POINT('',(-0.871530771444223,-0.04763,0.528110872004958));
#10537=CARTESIAN_POINT('Ctrl Pts',(-0.528110872004958,-0.0476300000000001,
0.871530771444223));
#10538=CARTESIAN_POINT('Ctrl Pts',(-0.530395067942936,-0.0609922781173484,
0.87014664509073));
#10539=CARTESIAN_POINT('Ctrl Pts',(-0.533674141594226,-0.0742967091364493,
0.868149331745851));
#10540=CARTESIAN_POINT('Ctrl Pts',(-0.54708917182331,-0.115492077056649,
0.85981294420286));
#10541=CARTESIAN_POINT('Ctrl Pts',(-0.560922177770136,-0.141695629206859,
0.850993704737257));
#10542=CARTESIAN_POINT('Ctrl Pts',(-0.590422647829571,-0.181890537957859,
0.830754510485543));
#10543=CARTESIAN_POINT('Ctrl Pts',(-0.609616703125488,-0.201072148666545,
0.816896541396381));
#10544=CARTESIAN_POINT('Ctrl Pts',(-0.641117951819998,-0.223955109275652,
0.792310597819928));
#10545=CARTESIAN_POINT('Ctrl Pts',(-0.657208095763053,-0.232742381310829,
0.779109323683611));
#10546=CARTESIAN_POINT('Ctrl Pts',(-0.68964083160521,-0.244234834628584,
0.750552691816205));
#10547=CARTESIAN_POINT('Ctrl Pts',(-0.705971972091755,-0.246942143572133,
0.735185187071673));
#10548=CARTESIAN_POINT('Ctrl Pts',(-0.735185187071673,-0.246942143572133,
0.705971972091754));
#10549=CARTESIAN_POINT('Ctrl Pts',(-0.750552691816206,-0.244234834628584,
0.689640831605209));
#10550=CARTESIAN_POINT('Ctrl Pts',(-0.779109323683612,-0.232742381310829,
0.657208095763052));
#10551=CARTESIAN_POINT('Ctrl Pts',(-0.792310597819928,-0.223955109275652,
0.641117951819998));
#10552=CARTESIAN_POINT('Ctrl Pts',(-0.816896541396382,-0.201072148666545,
0.609616703125487));
#10553=CARTESIAN_POINT('Ctrl Pts',(-0.830754510485544,-0.181890537957858,
0.590422647829571));
#10554=CARTESIAN_POINT('Ctrl Pts',(-0.850993704737257,-0.141695629206858,
0.560922177770135));
#10555=CARTESIAN_POINT('Ctrl Pts',(-0.859812944202861,-0.115492077056649,
0.547089171823309));
#10556=CARTESIAN_POINT('Ctrl Pts',(-0.868149331745852,-0.0742967091364491,
0.533674141594226));
#10557=CARTESIAN_POINT('Ctrl Pts',(-0.870146645090731,-0.0609922781173483,
0.530395067942936));
#10558=CARTESIAN_POINT('Ctrl Pts',(-0.871530771444223,-0.04763,0.528110872004958));
#10559=CARTESIAN_POINT('',(-0.989696097314,-0.04763,0.242834539687906));
#10560=CARTESIAN_POINT('Origin',(0.,-0.04763,0.));
#10561=CARTESIAN_POINT('',(-1.019052,-0.246942143572133,1.248489836334E-16));
#10562=CARTESIAN_POINT('Ctrl Pts',(-0.989696097314,-0.04763,0.242834539687906));
#10563=CARTESIAN_POINT('Ctrl Pts',(-0.990332542620729,-0.0609922781173483,
0.24024064412003));
#10564=CARTESIAN_POINT('Ctrl Pts',(-0.991238884025248,-0.0742967091364492,
0.236509675094874));
#10565=CARTESIAN_POINT('Ctrl Pts',(-0.994830026707808,-0.115492077056649,
0.221129100087819));
#10566=CARTESIAN_POINT('Ctrl Pts',(-0.998375294985966,-0.141695629206859,
0.205111543747588));
#10567=CARTESIAN_POINT('Ctrl Pts',(-1.00492400591205,-0.181890537957859,
0.169940289819232));
#10568=CARTESIAN_POINT('Ctrl Pts',(-1.00869718865384,-0.201072148666545,
0.1465689792446));
#10569=CARTESIAN_POINT('Ctrl Pts',(-1.01358704779679,-0.223955109275652,
0.106909345252088));
#10570=CARTESIAN_POINT('Ctrl Pts',(-1.0156297872271,-0.232742381310829,
0.0861971848975944));
#10571=CARTESIAN_POINT('Ctrl Pts',(-1.01837060663223,-0.244234834628584,
0.0430711894098825));
#10572=CARTESIAN_POINT('Ctrl Pts',(-1.019052,-0.246942143572133,0.0206568624125608));
#10573=CARTESIAN_POINT('Ctrl Pts',(-1.019052,-0.246942143572133,1.2490009027033E-16));
#10574=CARTESIAN_POINT('',(-1.019052,-0.28578,1.24797876996471E-16));
#10575=CARTESIAN_POINT('',(-1.019052,-0.166705,1.24797876996471E-16));
#10576=CARTESIAN_POINT('Origin',(0.,-0.28578,0.));
#10577=CARTESIAN_POINT('',(-0.989696097314,-0.04763,-0.242834539687906));
#10578=CARTESIAN_POINT('Ctrl Pts',(-1.019052,-0.246942143572133,1.2490009027033E-16));
#10579=CARTESIAN_POINT('Ctrl Pts',(-1.019052,-0.246942143572133,-0.0206568624125605));
#10580=CARTESIAN_POINT('Ctrl Pts',(-1.01837060663223,-0.244234834628584,
-0.0430711894098822));
#10581=CARTESIAN_POINT('Ctrl Pts',(-1.0156297872271,-0.232742381310829,
-0.0861971848975941));
#10582=CARTESIAN_POINT('Ctrl Pts',(-1.01358704779679,-0.223955109275652,
-0.106909345252087));
#10583=CARTESIAN_POINT('Ctrl Pts',(-1.00869718865384,-0.201072148666546,
-0.1465689792446));
#10584=CARTESIAN_POINT('Ctrl Pts',(-1.00492400591205,-0.181890537957859,
-0.169940289819232));
#10585=CARTESIAN_POINT('Ctrl Pts',(-0.998375294985966,-0.141695629206859,
-0.205111543747588));
#10586=CARTESIAN_POINT('Ctrl Pts',(-0.994830026707808,-0.11549207705665,
-0.221129100087819));
#10587=CARTESIAN_POINT('Ctrl Pts',(-0.991238884025248,-0.0742967091364495,
-0.236509675094874));
#10588=CARTESIAN_POINT('Ctrl Pts',(-0.990332542620729,-0.0609922781173484,
-0.24024064412003));
#10589=CARTESIAN_POINT('Ctrl Pts',(-0.989696097314,-0.0476300000000001,
-0.242834539687907));
#10590=CARTESIAN_POINT('',(-0.871530771444223,-0.04763,-0.528110872004958));
#10591=CARTESIAN_POINT('Origin',(0.,-0.04763,0.));
#10592=CARTESIAN_POINT('',(-0.528110872004958,-0.04763,-0.871530771444223));
#10593=CARTESIAN_POINT('Ctrl Pts',(-0.871530771444223,-0.0476300000000001,
-0.528110872004958));
#10594=CARTESIAN_POINT('Ctrl Pts',(-0.87014664509073,-0.0609922781173484,
-0.530395067942936));
#10595=CARTESIAN_POINT('Ctrl Pts',(-0.868149331745851,-0.0742967091364494,
-0.533674141594226));
#10596=CARTESIAN_POINT('Ctrl Pts',(-0.85981294420286,-0.115492077056649,
-0.54708917182331));
#10597=CARTESIAN_POINT('Ctrl Pts',(-0.850993704737257,-0.141695629206859,
-0.560922177770136));
#10598=CARTESIAN_POINT('Ctrl Pts',(-0.830754510485543,-0.181890537957859,
-0.590422647829571));
#10599=CARTESIAN_POINT('Ctrl Pts',(-0.816896541396381,-0.201072148666546,
-0.609616703125488));
#10600=CARTESIAN_POINT('Ctrl Pts',(-0.792310597819928,-0.223955109275652,
-0.641117951819999));
#10601=CARTESIAN_POINT('Ctrl Pts',(-0.779109323683611,-0.232742381310829,
-0.657208095763053));
#10602=CARTESIAN_POINT('Ctrl Pts',(-0.750552691816205,-0.244234834628584,
-0.68964083160521));
#10603=CARTESIAN_POINT('Ctrl Pts',(-0.735185187071673,-0.246942143572133,
-0.705971972091755));
#10604=CARTESIAN_POINT('Ctrl Pts',(-0.705971972091754,-0.246942143572133,
-0.735185187071673));
#10605=CARTESIAN_POINT('Ctrl Pts',(-0.68964083160521,-0.244234834628584,
-0.750552691816206));
#10606=CARTESIAN_POINT('Ctrl Pts',(-0.657208095763052,-0.232742381310829,
-0.779109323683612));
#10607=CARTESIAN_POINT('Ctrl Pts',(-0.641117951819998,-0.223955109275652,
-0.792310597819928));
#10608=CARTESIAN_POINT('Ctrl Pts',(-0.609616703125488,-0.201072148666545,
-0.816896541396381));
#10609=CARTESIAN_POINT('Ctrl Pts',(-0.590422647829571,-0.181890537957859,
-0.830754510485543));
#10610=CARTESIAN_POINT('Ctrl Pts',(-0.560922177770136,-0.141695629206859,
-0.850993704737257));
#10611=CARTESIAN_POINT('Ctrl Pts',(-0.54708917182331,-0.115492077056649,
-0.85981294420286));
#10612=CARTESIAN_POINT('Ctrl Pts',(-0.533674141594226,-0.0742967091364494,
-0.868149331745852));
#10613=CARTESIAN_POINT('Ctrl Pts',(-0.530395067942936,-0.0609922781173484,
-0.870146645090731));
#10614=CARTESIAN_POINT('Ctrl Pts',(-0.528110872004958,-0.0476300000000001,
-0.871530771444223));
#10615=CARTESIAN_POINT('',(-0.242834539687906,-0.04763,-0.989696097314));
#10616=CARTESIAN_POINT('Origin',(0.,-0.04763,0.));
#10617=CARTESIAN_POINT('',(0.242834539687906,-0.04763,-0.989696097314));
#10618=CARTESIAN_POINT('Ctrl Pts',(-0.242834539687907,-0.04763,-0.989696097314));
#10619=CARTESIAN_POINT('Ctrl Pts',(-0.24024064412003,-0.0609922781173483,
-0.990332542620729));
#10620=CARTESIAN_POINT('Ctrl Pts',(-0.236509675094874,-0.0742967091364493,
-0.991238884025248));
#10621=CARTESIAN_POINT('Ctrl Pts',(-0.221129100087819,-0.115492077056649,
-0.994830026707808));
#10622=CARTESIAN_POINT('Ctrl Pts',(-0.205111543747588,-0.141695629206859,
-0.998375294985966));
#10623=CARTESIAN_POINT('Ctrl Pts',(-0.169940289819232,-0.181890537957859,
-1.00492400591205));
#10624=CARTESIAN_POINT('Ctrl Pts',(-0.1465689792446,-0.201072148666545,
-1.00869718865384));
#10625=CARTESIAN_POINT('Ctrl Pts',(-0.106909345252087,-0.223955109275652,
-1.01358704779679));
#10626=CARTESIAN_POINT('Ctrl Pts',(-0.0861971848975942,-0.232742381310829,
-1.0156297872271));
#10627=CARTESIAN_POINT('Ctrl Pts',(-0.0430711894098823,-0.244234834628584,
-1.01837060663223));
#10628=CARTESIAN_POINT('Ctrl Pts',(-0.0206568624125606,-0.246942143572133,
-1.019052));
#10629=CARTESIAN_POINT('Ctrl Pts',(0.0206568624125607,-0.246942143572133,
-1.019052));
#10630=CARTESIAN_POINT('Ctrl Pts',(0.0430711894098824,-0.244234834628584,
-1.01837060663223));
#10631=CARTESIAN_POINT('Ctrl Pts',(0.0861971848975943,-0.232742381310829,
-1.0156297872271));
#10632=CARTESIAN_POINT('Ctrl Pts',(0.106909345252088,-0.223955109275652,
-1.01358704779679));
#10633=CARTESIAN_POINT('Ctrl Pts',(0.1465689792446,-0.201072148666545,-1.00869718865384));
#10634=CARTESIAN_POINT('Ctrl Pts',(0.169940289819232,-0.181890537957859,
-1.00492400591205));
#10635=CARTESIAN_POINT('Ctrl Pts',(0.205111543747588,-0.141695629206859,
-0.998375294985966));
#10636=CARTESIAN_POINT('Ctrl Pts',(0.221129100087819,-0.115492077056649,
-0.994830026707808));
#10637=CARTESIAN_POINT('Ctrl Pts',(0.236509675094874,-0.0742967091364493,
-0.991238884025248));
#10638=CARTESIAN_POINT('Ctrl Pts',(0.24024064412003,-0.0609922781173484,
-0.990332542620729));
#10639=CARTESIAN_POINT('Ctrl Pts',(0.242834539687907,-0.04763,-0.989696097314));
#10640=CARTESIAN_POINT('',(0.528110872004958,-0.04763,-0.871530771444223));
#10641=CARTESIAN_POINT('Origin',(0.,-0.04763,0.));
#10642=CARTESIAN_POINT('',(0.871530771444223,-0.04763,-0.528110872004958));
#10643=CARTESIAN_POINT('Ctrl Pts',(0.528110872004958,-0.0476300000000001,
-0.871530771444223));
#10644=CARTESIAN_POINT('Ctrl Pts',(0.530395067942936,-0.0609922781173484,
-0.870146645090731));
#10645=CARTESIAN_POINT('Ctrl Pts',(0.533674141594226,-0.0742967091364493,
-0.868149331745851));
#10646=CARTESIAN_POINT('Ctrl Pts',(0.54708917182331,-0.115492077056649,
-0.85981294420286));
#10647=CARTESIAN_POINT('Ctrl Pts',(0.560922177770136,-0.141695629206859,
-0.850993704737257));
#10648=CARTESIAN_POINT('Ctrl Pts',(0.590422647829571,-0.181890537957859,
-0.830754510485543));
#10649=CARTESIAN_POINT('Ctrl Pts',(0.609616703125488,-0.201072148666545,
-0.816896541396381));
#10650=CARTESIAN_POINT('Ctrl Pts',(0.641117951819998,-0.223955109275652,
-0.792310597819928));
#10651=CARTESIAN_POINT('Ctrl Pts',(0.657208095763053,-0.232742381310829,
-0.779109323683612));
#10652=CARTESIAN_POINT('Ctrl Pts',(0.68964083160521,-0.244234834628584,
-0.750552691816206));
#10653=CARTESIAN_POINT('Ctrl Pts',(0.705971972091755,-0.246942143572133,
-0.735185187071673));
#10654=CARTESIAN_POINT('Ctrl Pts',(0.735185187071673,-0.246942143572133,
-0.705971972091754));
#10655=CARTESIAN_POINT('Ctrl Pts',(0.750552691816206,-0.244234834628584,
-0.68964083160521));
#10656=CARTESIAN_POINT('Ctrl Pts',(0.779109323683612,-0.232742381310829,
-0.657208095763053));
#10657=CARTESIAN_POINT('Ctrl Pts',(0.792310597819928,-0.223955109275652,
-0.641117951819998));
#10658=CARTESIAN_POINT('Ctrl Pts',(0.816896541396381,-0.201072148666545,
-0.609616703125488));
#10659=CARTESIAN_POINT('Ctrl Pts',(0.830754510485543,-0.181890537957859,
-0.590422647829571));
#10660=CARTESIAN_POINT('Ctrl Pts',(0.850993704737257,-0.141695629206859,
-0.560922177770136));
#10661=CARTESIAN_POINT('Ctrl Pts',(0.85981294420286,-0.115492077056649,
-0.54708917182331));
#10662=CARTESIAN_POINT('Ctrl Pts',(0.868149331745851,-0.0742967091364493,
-0.533674141594226));
#10663=CARTESIAN_POINT('Ctrl Pts',(0.870146645090731,-0.0609922781173484,
-0.530395067942936));
#10664=CARTESIAN_POINT('Ctrl Pts',(0.871530771444223,-0.0476300000000001,
-0.528110872004958));
#10665=CARTESIAN_POINT('',(0.989696097314,-0.04763,-0.242834539687906));
#10666=CARTESIAN_POINT('Origin',(0.,-0.04763,0.));
#10667=CARTESIAN_POINT('',(0.989696097314,-0.04763,0.242834539687906));
#10668=CARTESIAN_POINT('Ctrl Pts',(0.989696097314,-0.04763,-0.242834539687907));
#10669=CARTESIAN_POINT('Ctrl Pts',(0.990332542620729,-0.0609922781173483,
-0.24024064412003));
#10670=CARTESIAN_POINT('Ctrl Pts',(0.991238884025248,-0.0742967091364493,
-0.236509675094874));
#10671=CARTESIAN_POINT('Ctrl Pts',(0.994830026707808,-0.115492077056649,
-0.221129100087819));
#10672=CARTESIAN_POINT('Ctrl Pts',(0.998375294985966,-0.141695629206859,
-0.205111543747588));
#10673=CARTESIAN_POINT('Ctrl Pts',(1.00492400591205,-0.181890537957859,
-0.169940289819232));
#10674=CARTESIAN_POINT('Ctrl Pts',(1.00869718865384,-0.201072148666545,
-0.1465689792446));
#10675=CARTESIAN_POINT('Ctrl Pts',(1.01358704779679,-0.223955109275652,
-0.106909345252087));
#10676=CARTESIAN_POINT('Ctrl Pts',(1.0156297872271,-0.232742381310829,-0.0861971848975942));
#10677=CARTESIAN_POINT('Ctrl Pts',(1.01837060663223,-0.244234834628584,
-0.0430711894098823));
#10678=CARTESIAN_POINT('Ctrl Pts',(1.019052,-0.246942143572133,-0.0206568624125607));
#10679=CARTESIAN_POINT('Ctrl Pts',(1.019052,-0.246942143572133,0.0206568624125607));
#10680=CARTESIAN_POINT('Ctrl Pts',(1.01837060663223,-0.244234834628584,
0.0430711894098823));
#10681=CARTESIAN_POINT('Ctrl Pts',(1.0156297872271,-0.232742381310829,0.0861971848975942));
#10682=CARTESIAN_POINT('Ctrl Pts',(1.01358704779679,-0.223955109275652,
0.106909345252087));
#10683=CARTESIAN_POINT('Ctrl Pts',(1.00869718865384,-0.201072148666545,
0.1465689792446));
#10684=CARTESIAN_POINT('Ctrl Pts',(1.00492400591205,-0.181890537957859,
0.169940289819232));
#10685=CARTESIAN_POINT('Ctrl Pts',(0.998375294985966,-0.141695629206859,
0.205111543747588));
#10686=CARTESIAN_POINT('Ctrl Pts',(0.994830026707808,-0.115492077056649,
0.221129100087819));
#10687=CARTESIAN_POINT('Ctrl Pts',(0.991238884025248,-0.0742967091364492,
0.236509675094874));
#10688=CARTESIAN_POINT('Ctrl Pts',(0.990332542620729,-0.0609922781173483,
0.24024064412003));
#10689=CARTESIAN_POINT('Ctrl Pts',(0.989696097314,-0.04763,0.242834539687907));
#10690=CARTESIAN_POINT('Origin',(0.,-0.04763,0.));
#10691=CARTESIAN_POINT('Origin',(0.,-0.04763,0.));
#10692=CARTESIAN_POINT('',(0.238183666596899,-0.04763,0.951592097314));
#10693=CARTESIAN_POINT('Origin',(0.,-0.04763,0.));
#10694=CARTESIAN_POINT('Origin',(-1.94289029309402E-16,-0.04763,1.));
#10695=CARTESIAN_POINT('Origin',(-1.94289029309402E-16,0.,1.));
#10696=CARTESIAN_POINT('',(-0.2381836665969,-0.04763,0.951592097314));
#10697=CARTESIAN_POINT('Ctrl Pts',(-0.238183666596899,-0.0476299999999999,
0.951592097314));
#10698=CARTESIAN_POINT('Ctrl Pts',(-0.233157223576062,-0.0740444353928835,
0.952850216871763));
#10699=CARTESIAN_POINT('Ctrl Pts',(-0.223801617934946,-0.0999305678883309,
0.955173119738174));
#10700=CARTESIAN_POINT('Ctrl Pts',(-0.199966927975188,-0.142345102874864,
0.960411259488514));
#10701=CARTESIAN_POINT('Ctrl Pts',(-0.1868781821531,-0.159766064500479,
0.963103647174702));
#10702=CARTESIAN_POINT('Ctrl Pts',(-0.15681442133453,-0.190326085855194,
0.968453058988463));
#10703=CARTESIAN_POINT('Ctrl Pts',(-0.139836317888043,-0.203463743702801,
0.971100730005489));
#10704=CARTESIAN_POINT('Ctrl Pts',(-0.104422493053067,-0.224161999508995,
0.975530745318961));
#10705=CARTESIAN_POINT('Ctrl Pts',(-0.0842175114474176,-0.232861760990032,
0.977553872336861));
#10706=CARTESIAN_POINT('Ctrl Pts',(-0.0421062857595701,-0.244251601209411,
0.980270995488453));
#10707=CARTESIAN_POINT('Ctrl Pts',(-0.0201990724523197,-0.246942143572133,
0.980948));
#10708=CARTESIAN_POINT('Ctrl Pts',(0.020199072452319,-0.246942143572133,
0.980948));
#10709=CARTESIAN_POINT('Ctrl Pts',(0.0421062857595694,-0.244251601209411,
0.980270995488454));
#10710=CARTESIAN_POINT('Ctrl Pts',(0.0842175114474169,-0.232861760990032,
0.977553872336861));
#10711=CARTESIAN_POINT('Ctrl Pts',(0.104422493053067,-0.224161999508995,
0.975530745318961));
#10712=CARTESIAN_POINT('Ctrl Pts',(0.139836317888042,-0.203463743702801,
0.971100730005489));
#10713=CARTESIAN_POINT('Ctrl Pts',(0.15681442133453,-0.190326085855194,
0.968453058988463));
#10714=CARTESIAN_POINT('Ctrl Pts',(0.1868781821531,-0.15976606450048,0.963103647174702));
#10715=CARTESIAN_POINT('Ctrl Pts',(0.199966927975188,-0.142345102874864,
0.960411259488514));
#10716=CARTESIAN_POINT('Ctrl Pts',(0.223801617934945,-0.0999305678883309,
0.955173119738174));
#10717=CARTESIAN_POINT('Ctrl Pts',(0.233157223576061,-0.0740444353928835,
0.952850216871763));
#10718=CARTESIAN_POINT('Ctrl Pts',(0.238183666596899,-0.0476299999999999,
0.951592097314));
#10719=CARTESIAN_POINT('Origin',(-1.94289029309402E-16,-0.04763,1.));
#10720=CARTESIAN_POINT('Origin',(0.,-0.04763,0.));
#10721=CARTESIAN_POINT('',(-0.504455939115715,-0.04763,0.841298510752802));
#10722=CARTESIAN_POINT('Origin',(0.,-0.04763,0.));
#10723=CARTESIAN_POINT('Origin',(-0.707106781186548,-0.04763,0.707106781186547));
#10724=CARTESIAN_POINT('Origin',(-0.707106781186548,0.,0.707106781186547));
#10725=CARTESIAN_POINT('',(-0.841298510752802,-0.04763,0.504455939115715));
#10726=CARTESIAN_POINT('Ctrl Pts',(-0.841298510752802,-0.04763,0.504455939115715));
#10727=CARTESIAN_POINT('Ctrl Pts',(-0.838633903678357,-0.0740444353928835,
0.508899795931835));
#10728=CARTESIAN_POINT('Ctrl Pts',(-0.833661031856294,-0.0999305678883309,
0.517157748491652));
#10729=CARTESIAN_POINT('Ctrl Pts',(-0.820511285096538,-0.142345102874864,
0.537715343527944));
#10730=CARTESIAN_POINT('Ctrl Pts',(-0.813159949759,-0.159766064500479,0.548874290046456));
#10731=CARTESIAN_POINT('Ctrl Pts',(-0.795684265985089,-0.190326085855194,
0.573915184558107));
#10732=CARTESIAN_POINT('Ctrl Pts',(-0.78555112003688,-0.203463743702801,
0.587792702767295));
#10733=CARTESIAN_POINT('Ctrl Pts',(-0.763642258217233,-0.224161999508995,
0.615966552324775));
#10734=CARTESIAN_POINT('Ctrl Pts',(-0.750785745543687,-0.232861760990032,
0.631684198665438));
#10735=CARTESIAN_POINT('Ctrl Pts',(-0.722929908501543,-0.244251601209411,
0.663382628119203));
#10736=CARTESIAN_POINT('Ctrl Pts',(-0.707917883896095,-0.246942143572133,
0.679352081686668));
#10737=CARTESIAN_POINT('Ctrl Pts',(-0.679352081686668,-0.246942143572133,
0.707917883896095));
#10738=CARTESIAN_POINT('Ctrl Pts',(-0.663382628119203,-0.244251601209411,
0.722929908501544));
#10739=CARTESIAN_POINT('Ctrl Pts',(-0.631684198665438,-0.232861760990031,
0.750785745543687));
#10740=CARTESIAN_POINT('Ctrl Pts',(-0.615966552324775,-0.224161999508995,
0.763642258217233));
#10741=CARTESIAN_POINT('Ctrl Pts',(-0.587792702767295,-0.203463743702801,
0.78555112003688));
#10742=CARTESIAN_POINT('Ctrl Pts',(-0.573915184558107,-0.190326085855194,
0.795684265985088));
#10743=CARTESIAN_POINT('Ctrl Pts',(-0.548874290046456,-0.159766064500479,
0.813159949759));
#10744=CARTESIAN_POINT('Ctrl Pts',(-0.537715343527944,-0.142345102874864,
0.820511285096538));
#10745=CARTESIAN_POINT('Ctrl Pts',(-0.517157748491652,-0.0999305678883309,
0.833661031856294));
#10746=CARTESIAN_POINT('Ctrl Pts',(-0.508899795931835,-0.0740444353928835,
0.838633903678357));
#10747=CARTESIAN_POINT('Ctrl Pts',(-0.504455939115716,-0.04763,0.841298510752801));
#10748=CARTESIAN_POINT('Origin',(-0.707106781186548,-0.04763,0.707106781186547));
#10749=CARTESIAN_POINT('Origin',(0.,-0.04763,0.));
#10750=CARTESIAN_POINT('',(-0.951592097314,-0.04763,0.238183666596899));
#10751=CARTESIAN_POINT('Origin',(0.,-0.04763,0.));
#10752=CARTESIAN_POINT('Origin',(-1.,-0.04763,-1.11022302462516E-16));
#10753=CARTESIAN_POINT('Origin',(-1.,0.,-1.11022302462516E-16));
#10754=CARTESIAN_POINT('',(-0.951592097314,-0.04763,-0.2381836665969));
#10755=CARTESIAN_POINT('',(-0.980948,-0.246942143572133,1.08514323328844E-18));
#10756=CARTESIAN_POINT('Ctrl Pts',(-0.951592097314,-0.04763,-0.238183666596899));
#10757=CARTESIAN_POINT('Ctrl Pts',(-0.952850216871763,-0.0740444353928835,
-0.233157223576062));
#10758=CARTESIAN_POINT('Ctrl Pts',(-0.955173119738174,-0.0999305678883309,
-0.223801617934946));
#10759=CARTESIAN_POINT('Ctrl Pts',(-0.960411259488514,-0.142345102874864,
-0.199966927975188));
#10760=CARTESIAN_POINT('Ctrl Pts',(-0.963103647174702,-0.159766064500479,
-0.1868781821531));
#10761=CARTESIAN_POINT('Ctrl Pts',(-0.968453058988463,-0.190326085855194,
-0.15681442133453));
#10762=CARTESIAN_POINT('Ctrl Pts',(-0.971100730005489,-0.203463743702801,
-0.139836317888043));
#10763=CARTESIAN_POINT('Ctrl Pts',(-0.975530745318961,-0.224161999508995,
-0.104422493053067));
#10764=CARTESIAN_POINT('Ctrl Pts',(-0.977553872336861,-0.232861760990032,
-0.0842175114474175));
#10765=CARTESIAN_POINT('Ctrl Pts',(-0.980270995488453,-0.244251601209411,
-0.0421062857595699));
#10766=CARTESIAN_POINT('Ctrl Pts',(-0.980948,-0.246942143572133,-0.0201990724523195));
#10767=CARTESIAN_POINT('Ctrl Pts',(-0.980948,-0.246942143572133,-1.17961196366423E-16));
#10768=CARTESIAN_POINT('Origin',(-1.,-0.04763,-1.11022302462516E-16));
#10769=CARTESIAN_POINT('Ctrl Pts',(-0.980948,-0.246942143572133,-1.17961196366423E-16));
#10770=CARTESIAN_POINT('Ctrl Pts',(-0.980948,-0.246942143572133,0.0201990724523192));
#10771=CARTESIAN_POINT('Ctrl Pts',(-0.980270995488453,-0.244251601209411,
0.0421062857595695));
#10772=CARTESIAN_POINT('Ctrl Pts',(-0.977553872336861,-0.232861760990032,
0.0842175114474169));
#10773=CARTESIAN_POINT('Ctrl Pts',(-0.975530745318961,-0.224161999508995,
0.104422493053066));
#10774=CARTESIAN_POINT('Ctrl Pts',(-0.971100730005489,-0.203463743702801,
0.139836317888042));
#10775=CARTESIAN_POINT('Ctrl Pts',(-0.968453058988463,-0.190326085855194,
0.15681442133453));
#10776=CARTESIAN_POINT('Ctrl Pts',(-0.963103647174702,-0.15976606450048,
0.1868781821531));
#10777=CARTESIAN_POINT('Ctrl Pts',(-0.960411259488514,-0.142345102874864,
0.199966927975188));
#10778=CARTESIAN_POINT('Ctrl Pts',(-0.955173119738174,-0.099930567888331,
0.223801617934945));
#10779=CARTESIAN_POINT('Ctrl Pts',(-0.952850216871763,-0.0740444353928835,
0.233157223576061));
#10780=CARTESIAN_POINT('Ctrl Pts',(-0.951592097314,-0.04763,0.238183666596899));
#10781=CARTESIAN_POINT('Origin',(0.,-0.04763,0.));
#10782=CARTESIAN_POINT('',(-0.841298510752802,-0.04763,-0.504455939115715));
#10783=CARTESIAN_POINT('Origin',(0.,-0.04763,0.));
#10784=CARTESIAN_POINT('Origin',(-0.707106781186547,-0.04763,-0.707106781186548));
#10785=CARTESIAN_POINT('Origin',(-0.707106781186547,0.,-0.707106781186548));
#10786=CARTESIAN_POINT('',(-0.504455939115715,-0.04763,-0.841298510752802));
#10787=CARTESIAN_POINT('Ctrl Pts',(-0.504455939115715,-0.04763,-0.841298510752802));
#10788=CARTESIAN_POINT('Ctrl Pts',(-0.508899795931835,-0.0740444353928835,
-0.838633903678357));
#10789=CARTESIAN_POINT('Ctrl Pts',(-0.517157748491652,-0.0999305678883309,
-0.833661031856294));
#10790=CARTESIAN_POINT('Ctrl Pts',(-0.537715343527944,-0.142345102874864,
-0.820511285096538));
#10791=CARTESIAN_POINT('Ctrl Pts',(-0.548874290046456,-0.159766064500479,
-0.813159949759));
#10792=CARTESIAN_POINT('Ctrl Pts',(-0.573915184558107,-0.190326085855194,
-0.795684265985089));
#10793=CARTESIAN_POINT('Ctrl Pts',(-0.587792702767295,-0.203463743702801,
-0.78555112003688));
#10794=CARTESIAN_POINT('Ctrl Pts',(-0.615966552324775,-0.224161999508995,
-0.763642258217233));
#10795=CARTESIAN_POINT('Ctrl Pts',(-0.631684198665438,-0.232861760990032,
-0.750785745543687));
#10796=CARTESIAN_POINT('Ctrl Pts',(-0.663382628119203,-0.244251601209411,
-0.722929908501543));
#10797=CARTESIAN_POINT('Ctrl Pts',(-0.679352081686668,-0.246942143572133,
-0.707917883896095));
#10798=CARTESIAN_POINT('Ctrl Pts',(-0.707917883896095,-0.246942143572133,
-0.679352081686668));
#10799=CARTESIAN_POINT('Ctrl Pts',(-0.722929908501543,-0.244251601209411,
-0.663382628119203));
#10800=CARTESIAN_POINT('Ctrl Pts',(-0.750785745543687,-0.232861760990032,
-0.631684198665439));
#10801=CARTESIAN_POINT('Ctrl Pts',(-0.763642258217232,-0.224161999508995,
-0.615966552324775));
#10802=CARTESIAN_POINT('Ctrl Pts',(-0.78555112003688,-0.203463743702801,
-0.587792702767295));
#10803=CARTESIAN_POINT('Ctrl Pts',(-0.795684265985088,-0.190326085855194,
-0.573915184558107));
#10804=CARTESIAN_POINT('Ctrl Pts',(-0.813159949759,-0.15976606450048,-0.548874290046456));
#10805=CARTESIAN_POINT('Ctrl Pts',(-0.820511285096538,-0.142345102874864,
-0.537715343527944));
#10806=CARTESIAN_POINT('Ctrl Pts',(-0.833661031856294,-0.0999305678883311,
-0.517157748491652));
#10807=CARTESIAN_POINT('Ctrl Pts',(-0.838633903678357,-0.0740444353928836,
-0.508899795931835));
#10808=CARTESIAN_POINT('Ctrl Pts',(-0.841298510752801,-0.04763,-0.504455939115715));
#10809=CARTESIAN_POINT('Origin',(-0.707106781186547,-0.04763,-0.707106781186548));
#10810=CARTESIAN_POINT('Origin',(0.,-0.04763,0.));
#10811=CARTESIAN_POINT('',(-0.238183666596899,-0.04763,-0.951592097314));
#10812=CARTESIAN_POINT('Origin',(0.,-0.04763,0.));
#10813=CARTESIAN_POINT('Origin',(5.55111512312578E-17,-0.04763,-1.));
#10814=CARTESIAN_POINT('Origin',(5.55111512312578E-17,0.,-1.));
#10815=CARTESIAN_POINT('',(0.238183666596899,-0.04763,-0.951592097314));
#10816=CARTESIAN_POINT('Ctrl Pts',(0.238183666596899,-0.04763,-0.951592097314));
#10817=CARTESIAN_POINT('Ctrl Pts',(0.233157223576062,-0.0740444353928835,
-0.952850216871763));
#10818=CARTESIAN_POINT('Ctrl Pts',(0.223801617934946,-0.099930567888331,
-0.955173119738174));
#10819=CARTESIAN_POINT('Ctrl Pts',(0.199966927975188,-0.142345102874864,
-0.960411259488514));
#10820=CARTESIAN_POINT('Ctrl Pts',(0.1868781821531,-0.15976606450048,-0.963103647174702));
#10821=CARTESIAN_POINT('Ctrl Pts',(0.15681442133453,-0.190326085855194,
-0.968453058988463));
#10822=CARTESIAN_POINT('Ctrl Pts',(0.139836317888042,-0.203463743702801,
-0.971100730005489));
#10823=CARTESIAN_POINT('Ctrl Pts',(0.104422493053067,-0.224161999508995,
-0.975530745318961));
#10824=CARTESIAN_POINT('Ctrl Pts',(0.0842175114474173,-0.232861760990032,
-0.977553872336861));
#10825=CARTESIAN_POINT('Ctrl Pts',(0.0421062857595698,-0.244251601209411,
-0.980270995488453));
#10826=CARTESIAN_POINT('Ctrl Pts',(0.0201990724523194,-0.246942143572133,
-0.980948));
#10827=CARTESIAN_POINT('Ctrl Pts',(-0.0201990724523193,-0.246942143572133,
-0.980948));
#10828=CARTESIAN_POINT('Ctrl Pts',(-0.0421062857595697,-0.244251601209411,
-0.980270995488453));
#10829=CARTESIAN_POINT('Ctrl Pts',(-0.0842175114474171,-0.232861760990032,
-0.977553872336861));
#10830=CARTESIAN_POINT('Ctrl Pts',(-0.104422493053067,-0.224161999508995,
-0.975530745318961));
#10831=CARTESIAN_POINT('Ctrl Pts',(-0.139836317888042,-0.203463743702801,
-0.971100730005489));
#10832=CARTESIAN_POINT('Ctrl Pts',(-0.15681442133453,-0.190326085855194,
-0.968453058988463));
#10833=CARTESIAN_POINT('Ctrl Pts',(-0.1868781821531,-0.15976606450048,-0.963103647174702));
#10834=CARTESIAN_POINT('Ctrl Pts',(-0.199966927975188,-0.142345102874864,
-0.960411259488514));
#10835=CARTESIAN_POINT('Ctrl Pts',(-0.223801617934945,-0.099930567888331,
-0.955173119738174));
#10836=CARTESIAN_POINT('Ctrl Pts',(-0.233157223576062,-0.0740444353928835,
-0.952850216871763));
#10837=CARTESIAN_POINT('Ctrl Pts',(-0.238183666596899,-0.0476299999999999,
-0.951592097314));
#10838=CARTESIAN_POINT('Origin',(5.55111512312578E-17,-0.04763,-1.));
#10839=CARTESIAN_POINT('Origin',(0.,-0.04763,0.));
#10840=CARTESIAN_POINT('',(0.504455939115715,-0.04763,-0.841298510752802));
#10841=CARTESIAN_POINT('Origin',(0.,-0.04763,0.));
#10842=CARTESIAN_POINT('Origin',(0.707106781186548,-0.04763,-0.707106781186547));
#10843=CARTESIAN_POINT('Origin',(0.707106781186548,0.,-0.707106781186547));
#10844=CARTESIAN_POINT('',(0.841298510752802,-0.04763,-0.504455939115715));
#10845=CARTESIAN_POINT('Ctrl Pts',(0.841298510752802,-0.04763,-0.504455939115715));
#10846=CARTESIAN_POINT('Ctrl Pts',(0.838633903678357,-0.0740444353928835,
-0.508899795931835));
#10847=CARTESIAN_POINT('Ctrl Pts',(0.833661031856294,-0.0999305678883309,
-0.517157748491652));
#10848=CARTESIAN_POINT('Ctrl Pts',(0.820511285096538,-0.142345102874864,
-0.537715343527944));
#10849=CARTESIAN_POINT('Ctrl Pts',(0.813159949759,-0.159766064500479,-0.548874290046456));
#10850=CARTESIAN_POINT('Ctrl Pts',(0.795684265985088,-0.190326085855194,
-0.573915184558107));
#10851=CARTESIAN_POINT('Ctrl Pts',(0.78555112003688,-0.203463743702801,
-0.587792702767295));
#10852=CARTESIAN_POINT('Ctrl Pts',(0.763642258217233,-0.224161999508995,
-0.615966552324775));
#10853=CARTESIAN_POINT('Ctrl Pts',(0.750785745543687,-0.232861760990032,
-0.631684198665438));
#10854=CARTESIAN_POINT('Ctrl Pts',(0.722929908501543,-0.244251601209411,
-0.663382628119203));
#10855=CARTESIAN_POINT('Ctrl Pts',(0.707917883896095,-0.246942143572133,
-0.679352081686668));
#10856=CARTESIAN_POINT('Ctrl Pts',(0.679352081686668,-0.246942143572133,
-0.707917883896095));
#10857=CARTESIAN_POINT('Ctrl Pts',(0.663382628119203,-0.244251601209411,
-0.722929908501543));
#10858=CARTESIAN_POINT('Ctrl Pts',(0.631684198665438,-0.232861760990032,
-0.750785745543687));
#10859=CARTESIAN_POINT('Ctrl Pts',(0.615966552324775,-0.224161999508995,
-0.763642258217232));
#10860=CARTESIAN_POINT('Ctrl Pts',(0.587792702767295,-0.203463743702801,
-0.78555112003688));
#10861=CARTESIAN_POINT('Ctrl Pts',(0.573915184558107,-0.190326085855194,
-0.795684265985088));
#10862=CARTESIAN_POINT('Ctrl Pts',(0.548874290046456,-0.159766064500479,
-0.813159949759));
#10863=CARTESIAN_POINT('Ctrl Pts',(0.537715343527944,-0.142345102874864,
-0.820511285096538));
#10864=CARTESIAN_POINT('Ctrl Pts',(0.517157748491652,-0.099930567888331,
-0.833661031856294));
#10865=CARTESIAN_POINT('Ctrl Pts',(0.508899795931835,-0.0740444353928835,
-0.838633903678357));
#10866=CARTESIAN_POINT('Ctrl Pts',(0.504455939115715,-0.04763,-0.841298510752801));
#10867=CARTESIAN_POINT('Origin',(0.707106781186548,-0.04763,-0.707106781186547));
#10868=CARTESIAN_POINT('Origin',(0.,-0.166705,0.));
#10869=CARTESIAN_POINT('',(-0.980948,-0.28578,1.20131482833E-16));
#10870=CARTESIAN_POINT('Origin',(0.,-0.28578,0.));
#10871=CARTESIAN_POINT('',(-0.980948,-0.166705,1.20131482833E-16));
#10872=CARTESIAN_POINT('',(0.951592097314,-0.04763,0.238183666596899));
#10873=CARTESIAN_POINT('Origin',(0.,-0.04763,0.));
#10874=CARTESIAN_POINT('',(0.951592097314,-0.04763,-0.238183666596899));
#10875=CARTESIAN_POINT('Ctrl Pts',(0.951592097314,-0.04763,0.238183666596899));
#10876=CARTESIAN_POINT('Ctrl Pts',(0.952850216871763,-0.0740444353928835,
0.233157223576062));
#10877=CARTESIAN_POINT('Ctrl Pts',(0.955173119738174,-0.099930567888331,
0.223801617934945));
#10878=CARTESIAN_POINT('Ctrl Pts',(0.960411259488514,-0.142345102874864,
0.199966927975188));
#10879=CARTESIAN_POINT('Ctrl Pts',(0.963103647174702,-0.15976606450048,
0.1868781821531));
#10880=CARTESIAN_POINT('Ctrl Pts',(0.968453058988463,-0.190326085855194,
0.15681442133453));
#10881=CARTESIAN_POINT('Ctrl Pts',(0.971100730005489,-0.203463743702801,
0.139836317888042));
#10882=CARTESIAN_POINT('Ctrl Pts',(0.975530745318961,-0.224161999508995,
0.104422493053067));
#10883=CARTESIAN_POINT('Ctrl Pts',(0.977553872336861,-0.232861760990032,
0.0842175114474172));
#10884=CARTESIAN_POINT('Ctrl Pts',(0.980270995488453,-0.244251601209411,
0.0421062857595697));
#10885=CARTESIAN_POINT('Ctrl Pts',(0.980948,-0.246942143572133,0.0201990724523194));
#10886=CARTESIAN_POINT('Ctrl Pts',(0.980948,-0.246942143572133,-0.0201990724523194));
#10887=CARTESIAN_POINT('Ctrl Pts',(0.980270995488453,-0.244251601209411,
-0.0421062857595697));
#10888=CARTESIAN_POINT('Ctrl Pts',(0.977553872336861,-0.232861760990032,
-0.0842175114474172));
#10889=CARTESIAN_POINT('Ctrl Pts',(0.975530745318961,-0.224161999508995,
-0.104422493053067));
#10890=CARTESIAN_POINT('Ctrl Pts',(0.971100730005489,-0.203463743702801,
-0.139836317888042));
#10891=CARTESIAN_POINT('Ctrl Pts',(0.968453058988463,-0.190326085855194,
-0.15681442133453));
#10892=CARTESIAN_POINT('Ctrl Pts',(0.963103647174702,-0.15976606450048,
-0.1868781821531));
#10893=CARTESIAN_POINT('Ctrl Pts',(0.960411259488514,-0.142345102874864,
-0.199966927975188));
#10894=CARTESIAN_POINT('Ctrl Pts',(0.955173119738174,-0.099930567888331,
-0.223801617934945));
#10895=CARTESIAN_POINT('Ctrl Pts',(0.952850216871763,-0.0740444353928835,
-0.233157223576062));
#10896=CARTESIAN_POINT('Ctrl Pts',(0.951592097314,-0.0476299999999999,-0.238183666596899));
#10897=CARTESIAN_POINT('Origin',(0.,-0.04763,0.));
#10898=CARTESIAN_POINT('Origin',(0.,-0.04763,0.));
#10899=CARTESIAN_POINT('Origin',(1.,-0.04763,0.));
#10900=CARTESIAN_POINT('Origin',(1.,0.,0.));
#10901=CARTESIAN_POINT('Origin',(1.,-0.04763,0.));
#10902=CARTESIAN_POINT('Origin',(0.,-0.28578,0.));
#10903=CARTESIAN_POINT('Origin',(0.,-0.04763,0.));
#10904=CARTESIAN_POINT('',(0.,0.,0.));
#10905=CARTESIAN_POINT('Origin',(1.013815,0.445,0.));
#10906=CARTESIAN_POINT('',(-1.013815,0.445,-1.24156529467757E-16));
#10907=CARTESIAN_POINT('Origin',(0.,0.445,0.));
#10908=CARTESIAN_POINT('',(-0.991185,0.445,-1.21385153761287E-16));
#10909=CARTESIAN_POINT('Origin',(0.,0.445,0.));
#10910=CARTESIAN_POINT('Origin',(0.,0.4075,0.));
#10911=CARTESIAN_POINT('',(-1.013815,0.37,-1.24156529467757E-16));
#10912=CARTESIAN_POINT('Origin',(0.,0.37,0.));
#10913=CARTESIAN_POINT('',(-1.013815,0.4075,-1.24156529467757E-16));
#10914=CARTESIAN_POINT('Origin',(0.991185,0.37,0.));
#10915=CARTESIAN_POINT('',(-0.991185,0.37,-1.21385153761287E-16));
#10916=CARTESIAN_POINT('Origin',(0.,0.37,0.));
#10917=CARTESIAN_POINT('Origin',(0.,0.4075,0.));
#10918=CARTESIAN_POINT('',(-0.991185,0.4075,-1.21385153761287E-16));
#10919=CARTESIAN_POINT('Origin',(1.013815,-0.37,0.));
#10920=CARTESIAN_POINT('',(-1.013815,-0.37,-1.24156529467757E-16));
#10921=CARTESIAN_POINT('Origin',(0.,-0.37,0.));
#10922=CARTESIAN_POINT('',(-0.991185,-0.37,-1.21385153761287E-16));
#10923=CARTESIAN_POINT('Origin',(0.,-0.37,0.));
#10924=CARTESIAN_POINT('Origin',(0.,-0.4075,0.));
#10925=CARTESIAN_POINT('',(-1.013815,-0.445,-1.24156529467757E-16));
#10926=CARTESIAN_POINT('Origin',(0.,-0.445,0.));
#10927=CARTESIAN_POINT('',(-1.013815,-0.4075,-1.24156529467757E-16));
#10928=CARTESIAN_POINT('Origin',(0.991185,-0.445,0.));
#10929=CARTESIAN_POINT('',(-0.991185,-0.445,-1.21385153761287E-16));
#10930=CARTESIAN_POINT('Origin',(0.,-0.445,0.));
#10931=CARTESIAN_POINT('Origin',(0.,-0.4075,0.));
#10932=CARTESIAN_POINT('',(-0.991185,-0.4075,-1.21385153761287E-16));
#10933=CARTESIAN_POINT('',(0.,0.,0.));
#10934=CARTESIAN_POINT('',(0.,0.,0.));
#10935=CARTESIAN_POINT('',(0.,0.,0.));
#10936=CARTESIAN_POINT('',(0.,0.,0.));
#10937=CARTESIAN_POINT('',(0.,0.,0.));
#10938=CARTESIAN_POINT('',(0.,0.,0.));
#10939=CARTESIAN_POINT('',(0.,0.,0.));
#10940=CARTESIAN_POINT('',(0.,0.,0.));
#10941=CARTESIAN_POINT('',(0.,0.,0.));
#10942=CARTESIAN_POINT('',(0.,0.,0.));
#10943=CARTESIAN_POINT('',(0.,0.,0.));
#10944=CARTESIAN_POINT('',(0.,0.,0.));
#10945=CARTESIAN_POINT('',(0.,0.,2.5));
#10946=CARTESIAN_POINT('',(1.76776695296637,1.76776695296637,1.8));
#10947=CARTESIAN_POINT('',(1.23743686707646,1.23743686707646,4.));
#10948=CARTESIAN_POINT('',(-1.76776695296637,1.76776695296637,1.8));
#10949=CARTESIAN_POINT('',(-1.23743686707646,1.23743686707646,4.));
#10950=CARTESIAN_POINT('',(-1.76776695296637,-1.76776695296637,1.8));
#10951=CARTESIAN_POINT('',(-1.23743686707646,-1.23743686707646,4.));
#10952=CARTESIAN_POINT('',(1.76776695296637,-1.76776695296637,1.8));
#10953=CARTESIAN_POINT('',(1.23743686707646,-1.23743686707646,4.));
#10954=CARTESIAN_POINT('',(11.5,0.,5.25));
#10955=CARTESIAN_POINT('',(10.7,-1.5,2.));
#10956=CARTESIAN_POINT('',(10.7,1.5,2.));
#10957=CARTESIAN_POINT('',(9.7,-1.2,4.05));
#10958=CARTESIAN_POINT('',(9.7,-1.2,6.45));
#10959=CARTESIAN_POINT('',(9.7,1.2,4.05));
#10960=CARTESIAN_POINT('',(9.7,1.2,6.45));
#10961=CARTESIAN_POINT('',(13.3,-1.2,4.05));
#10962=CARTESIAN_POINT('',(13.3,-1.2,6.45));
#10963=CARTESIAN_POINT('',(13.3,1.2,4.05));
#10964=CARTESIAN_POINT('',(13.3,1.2,6.45));
#10965=CARTESIAN_POINT('',(4.,0.,5.25));
#10966=CARTESIAN_POINT('',(0.,0.,0.));
#10967=CARTESIAN_POINT('',(0.,0.,0.));
#10968=CARTESIAN_POINT('',(0.099999869213991,6.39097151088995E-80,-5.56755219029849E-32));
#10969=CARTESIAN_POINT('',(0.871405718515668,-2.36139361608283,-6.74166207035385E-14));
#10970=UNCERTAINTY_MEASURE_WITH_UNIT(LENGTH_MEASURE(0.001),#11036,
'DISTANCE_ACCURACY_VALUE',
'Maximum model space distance between geometric entities at asserted c
onnectivities');
#10971=UNCERTAINTY_MEASURE_WITH_UNIT(LENGTH_MEASURE(0.001),#11036,
'DISTANCE_ACCURACY_VALUE',
'Maximum model space distance between geometric entities at asserted c
onnectivities');
#10972=UNCERTAINTY_MEASURE_WITH_UNIT(LENGTH_MEASURE(0.001),#11036,
'DISTANCE_ACCURACY_VALUE',
'Maximum model space distance between geometric entities at asserted c
onnectivities');
#10973=UNCERTAINTY_MEASURE_WITH_UNIT(LENGTH_MEASURE(0.001),#11036,
'DISTANCE_ACCURACY_VALUE',
'Maximum model space distance between geometric entities at asserted c
onnectivities');
#10974=UNCERTAINTY_MEASURE_WITH_UNIT(LENGTH_MEASURE(0.001),#11036,
'DISTANCE_ACCURACY_VALUE',
'Maximum model space distance between geometric entities at asserted c
onnectivities');
#10975=UNCERTAINTY_MEASURE_WITH_UNIT(LENGTH_MEASURE(0.001),#11036,
'DISTANCE_ACCURACY_VALUE',
'Maximum model space distance between geometric entities at asserted c
onnectivities');
#10976=UNCERTAINTY_MEASURE_WITH_UNIT(LENGTH_MEASURE(0.001),#11036,
'DISTANCE_ACCURACY_VALUE',
'Maximum model space distance between geometric entities at asserted c
onnectivities');
#10977=UNCERTAINTY_MEASURE_WITH_UNIT(LENGTH_MEASURE(0.001),#11036,
'DISTANCE_ACCURACY_VALUE',
'Maximum model space distance between geometric entities at asserted c
onnectivities');
#10978=UNCERTAINTY_MEASURE_WITH_UNIT(LENGTH_MEASURE(0.001),#11036,
'DISTANCE_ACCURACY_VALUE',
'Maximum model space distance between geometric entities at asserted c
onnectivities');
#10979=UNCERTAINTY_MEASURE_WITH_UNIT(LENGTH_MEASURE(0.001),#11036,
'DISTANCE_ACCURACY_VALUE',
'Maximum model space distance between geometric entities at asserted c
onnectivities');
#10980=UNCERTAINTY_MEASURE_WITH_UNIT(LENGTH_MEASURE(0.001),#11036,
'DISTANCE_ACCURACY_VALUE',
'Maximum model space distance between geometric entities at asserted c
onnectivities');
#10981=UNCERTAINTY_MEASURE_WITH_UNIT(LENGTH_MEASURE(0.001),#11036,
'DISTANCE_ACCURACY_VALUE',
'Maximum model space distance between geometric entities at asserted c
onnectivities');
#10982=UNCERTAINTY_MEASURE_WITH_UNIT(LENGTH_MEASURE(0.001),#11036,
'DISTANCE_ACCURACY_VALUE',
'Maximum model space distance between geometric entities at asserted c
onnectivities');
#10983=UNCERTAINTY_MEASURE_WITH_UNIT(LENGTH_MEASURE(0.001),#11036,
'DISTANCE_ACCURACY_VALUE',
'Maximum model space distance between geometric entities at asserted c
onnectivities');
#10984=UNCERTAINTY_MEASURE_WITH_UNIT(LENGTH_MEASURE(0.001),#11036,
'DISTANCE_ACCURACY_VALUE',
'Maximum model space distance between geometric entities at asserted c
onnectivities');
#10985=UNCERTAINTY_MEASURE_WITH_UNIT(LENGTH_MEASURE(0.001),#11036,
'DISTANCE_ACCURACY_VALUE',
'Maximum model space distance between geometric entities at asserted c
onnectivities');
#10986=UNCERTAINTY_MEASURE_WITH_UNIT(LENGTH_MEASURE(0.001),#11036,
'DISTANCE_ACCURACY_VALUE',
'Maximum model space distance between geometric entities at asserted c
onnectivities');
#10987=UNCERTAINTY_MEASURE_WITH_UNIT(LENGTH_MEASURE(0.001),#11036,
'DISTANCE_ACCURACY_VALUE',
'Maximum model space distance between geometric entities at asserted c
onnectivities');
#10988=UNCERTAINTY_MEASURE_WITH_UNIT(LENGTH_MEASURE(0.001),#11036,
'DISTANCE_ACCURACY_VALUE',
'Maximum model space distance between geometric entities at asserted c
onnectivities');
#10989=UNCERTAINTY_MEASURE_WITH_UNIT(LENGTH_MEASURE(0.001),#11036,
'DISTANCE_ACCURACY_VALUE',
'Maximum model space distance between geometric entities at asserted c
onnectivities');
#10990=UNCERTAINTY_MEASURE_WITH_UNIT(LENGTH_MEASURE(0.001),#11036,
'DISTANCE_ACCURACY_VALUE',
'Maximum model space distance between geometric entities at asserted c
onnectivities');
#10991=UNCERTAINTY_MEASURE_WITH_UNIT(LENGTH_MEASURE(0.001),#11036,
'DISTANCE_ACCURACY_VALUE',
'Maximum model space distance between geometric entities at asserted c
onnectivities');
#10992=UNCERTAINTY_MEASURE_WITH_UNIT(LENGTH_MEASURE(0.001),#11036,
'DISTANCE_ACCURACY_VALUE',
'Maximum model space distance between geometric entities at asserted c
onnectivities');
#10993=UNCERTAINTY_MEASURE_WITH_UNIT(LENGTH_MEASURE(0.001),#11036,
'DISTANCE_ACCURACY_VALUE',
'Maximum model space distance between geometric entities at asserted c
onnectivities');
#10994=UNCERTAINTY_MEASURE_WITH_UNIT(LENGTH_MEASURE(0.001),#11036,
'DISTANCE_ACCURACY_VALUE',
'Maximum model space distance between geometric entities at asserted c
onnectivities');
#10995=UNCERTAINTY_MEASURE_WITH_UNIT(LENGTH_MEASURE(0.001),#11036,
'DISTANCE_ACCURACY_VALUE',
'Maximum model space distance between geometric entities at asserted c
onnectivities');
#10996=UNCERTAINTY_MEASURE_WITH_UNIT(LENGTH_MEASURE(0.001),#11036,
'DISTANCE_ACCURACY_VALUE',
'Maximum model space distance between geometric entities at asserted c
onnectivities');
#10997=UNCERTAINTY_MEASURE_WITH_UNIT(LENGTH_MEASURE(0.001),#11036,
'DISTANCE_ACCURACY_VALUE',
'Maximum model space distance between geometric entities at asserted c
onnectivities');
#10998=UNCERTAINTY_MEASURE_WITH_UNIT(LENGTH_MEASURE(0.001),#11036,
'DISTANCE_ACCURACY_VALUE',
'Maximum model space distance between geometric entities at asserted c
onnectivities');
#10999=UNCERTAINTY_MEASURE_WITH_UNIT(LENGTH_MEASURE(0.001),#11036,
'DISTANCE_ACCURACY_VALUE',
'Maximum model space distance between geometric entities at asserted c
onnectivities');
#11000=UNCERTAINTY_MEASURE_WITH_UNIT(LENGTH_MEASURE(0.001),#11036,
'DISTANCE_ACCURACY_VALUE',
'Maximum model space distance between geometric entities at asserted c
onnectivities');
#11001=UNCERTAINTY_MEASURE_WITH_UNIT(LENGTH_MEASURE(0.001),#11036,
'DISTANCE_ACCURACY_VALUE',
'Maximum model space distance between geometric entities at asserted c
onnectivities');
#11002=UNCERTAINTY_MEASURE_WITH_UNIT(LENGTH_MEASURE(0.001),#11036,
'DISTANCE_ACCURACY_VALUE',
'Maximum model space distance between geometric entities at asserted c
onnectivities');
#11003=(
GEOMETRIC_REPRESENTATION_CONTEXT(3)
GLOBAL_UNCERTAINTY_ASSIGNED_CONTEXT((#10970))
GLOBAL_UNIT_ASSIGNED_CONTEXT((#11036,#11038,#11039))
REPRESENTATION_CONTEXT('','3D')
);
#11004=(
GEOMETRIC_REPRESENTATION_CONTEXT(3)
GLOBAL_UNCERTAINTY_ASSIGNED_CONTEXT((#10971))
GLOBAL_UNIT_ASSIGNED_CONTEXT((#11036,#11038,#11039))
REPRESENTATION_CONTEXT('','3D')
);
#11005=(
GEOMETRIC_REPRESENTATION_CONTEXT(3)
GLOBAL_UNCERTAINTY_ASSIGNED_CONTEXT((#10972))
GLOBAL_UNIT_ASSIGNED_CONTEXT((#11036,#11038,#11039))
REPRESENTATION_CONTEXT('','3D')
);
#11006=(
GEOMETRIC_REPRESENTATION_CONTEXT(3)
GLOBAL_UNCERTAINTY_ASSIGNED_CONTEXT((#10973))
GLOBAL_UNIT_ASSIGNED_CONTEXT((#11036,#11038,#11039))
REPRESENTATION_CONTEXT('','3D')
);
#11007=(
GEOMETRIC_REPRESENTATION_CONTEXT(3)
GLOBAL_UNCERTAINTY_ASSIGNED_CONTEXT((#10974))
GLOBAL_UNIT_ASSIGNED_CONTEXT((#11036,#11038,#11039))
REPRESENTATION_CONTEXT('','3D')
);
#11008=(
GEOMETRIC_REPRESENTATION_CONTEXT(3)
GLOBAL_UNCERTAINTY_ASSIGNED_CONTEXT((#10975))
GLOBAL_UNIT_ASSIGNED_CONTEXT((#11036,#11038,#11039))
REPRESENTATION_CONTEXT('','3D')
);
#11009=(
GEOMETRIC_REPRESENTATION_CONTEXT(3)
GLOBAL_UNCERTAINTY_ASSIGNED_CONTEXT((#10976))
GLOBAL_UNIT_ASSIGNED_CONTEXT((#11036,#11038,#11039))
REPRESENTATION_CONTEXT('','3D')
);
#11010=(
GEOMETRIC_REPRESENTATION_CONTEXT(3)
GLOBAL_UNCERTAINTY_ASSIGNED_CONTEXT((#10977))
GLOBAL_UNIT_ASSIGNED_CONTEXT((#11036,#11038,#11039))
REPRESENTATION_CONTEXT('','3D')
);
#11011=(
GEOMETRIC_REPRESENTATION_CONTEXT(3)
GLOBAL_UNCERTAINTY_ASSIGNED_CONTEXT((#10978))
GLOBAL_UNIT_ASSIGNED_CONTEXT((#11036,#11038,#11039))
REPRESENTATION_CONTEXT('','3D')
);
#11012=(
GEOMETRIC_REPRESENTATION_CONTEXT(3)
GLOBAL_UNCERTAINTY_ASSIGNED_CONTEXT((#10979))
GLOBAL_UNIT_ASSIGNED_CONTEXT((#11036,#11038,#11039))
REPRESENTATION_CONTEXT('','3D')
);
#11013=(
GEOMETRIC_REPRESENTATION_CONTEXT(3)
GLOBAL_UNCERTAINTY_ASSIGNED_CONTEXT((#10980))
GLOBAL_UNIT_ASSIGNED_CONTEXT((#11036,#11038,#11039))
REPRESENTATION_CONTEXT('','3D')
);
#11014=(
GEOMETRIC_REPRESENTATION_CONTEXT(3)
GLOBAL_UNCERTAINTY_ASSIGNED_CONTEXT((#10981))
GLOBAL_UNIT_ASSIGNED_CONTEXT((#11036,#11038,#11039))
REPRESENTATION_CONTEXT('','3D')
);
#11015=(
GEOMETRIC_REPRESENTATION_CONTEXT(3)
GLOBAL_UNCERTAINTY_ASSIGNED_CONTEXT((#10982))
GLOBAL_UNIT_ASSIGNED_CONTEXT((#11036,#11038,#11039))
REPRESENTATION_CONTEXT('','3D')
);
#11016=(
GEOMETRIC_REPRESENTATION_CONTEXT(3)
GLOBAL_UNCERTAINTY_ASSIGNED_CONTEXT((#10983))
GLOBAL_UNIT_ASSIGNED_CONTEXT((#11036,#11038,#11039))
REPRESENTATION_CONTEXT('','3D')
);
#11017=(
GEOMETRIC_REPRESENTATION_CONTEXT(3)
GLOBAL_UNCERTAINTY_ASSIGNED_CONTEXT((#10984))
GLOBAL_UNIT_ASSIGNED_CONTEXT((#11036,#11038,#11039))
REPRESENTATION_CONTEXT('','3D')
);
#11018=(
GEOMETRIC_REPRESENTATION_CONTEXT(3)
GLOBAL_UNCERTAINTY_ASSIGNED_CONTEXT((#10985))
GLOBAL_UNIT_ASSIGNED_CONTEXT((#11036,#11038,#11039))
REPRESENTATION_CONTEXT('','3D')
);
#11019=(
GEOMETRIC_REPRESENTATION_CONTEXT(3)
GLOBAL_UNCERTAINTY_ASSIGNED_CONTEXT((#10986))
GLOBAL_UNIT_ASSIGNED_CONTEXT((#11036,#11038,#11039))
REPRESENTATION_CONTEXT('','3D')
);
#11020=(
GEOMETRIC_REPRESENTATION_CONTEXT(3)
GLOBAL_UNCERTAINTY_ASSIGNED_CONTEXT((#10987))
GLOBAL_UNIT_ASSIGNED_CONTEXT((#11036,#11038,#11039))
REPRESENTATION_CONTEXT('','3D')
);
#11021=(
GEOMETRIC_REPRESENTATION_CONTEXT(3)
GLOBAL_UNCERTAINTY_ASSIGNED_CONTEXT((#10988))
GLOBAL_UNIT_ASSIGNED_CONTEXT((#11036,#11038,#11039))
REPRESENTATION_CONTEXT('','3D')
);
#11022=(
GEOMETRIC_REPRESENTATION_CONTEXT(3)
GLOBAL_UNCERTAINTY_ASSIGNED_CONTEXT((#10989))
GLOBAL_UNIT_ASSIGNED_CONTEXT((#11036,#11038,#11039))
REPRESENTATION_CONTEXT('','3D')
);
#11023=(
GEOMETRIC_REPRESENTATION_CONTEXT(3)
GLOBAL_UNCERTAINTY_ASSIGNED_CONTEXT((#10990))
GLOBAL_UNIT_ASSIGNED_CONTEXT((#11036,#11038,#11039))
REPRESENTATION_CONTEXT('','3D')
);
#11024=(
GEOMETRIC_REPRESENTATION_CONTEXT(3)
GLOBAL_UNCERTAINTY_ASSIGNED_CONTEXT((#10991))
GLOBAL_UNIT_ASSIGNED_CONTEXT((#11036,#11038,#11039))
REPRESENTATION_CONTEXT('','3D')
);
#11025=(
GEOMETRIC_REPRESENTATION_CONTEXT(3)
GLOBAL_UNCERTAINTY_ASSIGNED_CONTEXT((#10992))
GLOBAL_UNIT_ASSIGNED_CONTEXT((#11036,#11038,#11039))
REPRESENTATION_CONTEXT('','3D')
);
#11026=(
GEOMETRIC_REPRESENTATION_CONTEXT(3)
GLOBAL_UNCERTAINTY_ASSIGNED_CONTEXT((#10993))
GLOBAL_UNIT_ASSIGNED_CONTEXT((#11036,#11038,#11039))
REPRESENTATION_CONTEXT('','3D')
);
#11027=(
GEOMETRIC_REPRESENTATION_CONTEXT(3)
GLOBAL_UNCERTAINTY_ASSIGNED_CONTEXT((#10994))
GLOBAL_UNIT_ASSIGNED_CONTEXT((#11036,#11038,#11039))
REPRESENTATION_CONTEXT('','3D')
);
#11028=(
GEOMETRIC_REPRESENTATION_CONTEXT(3)
GLOBAL_UNCERTAINTY_ASSIGNED_CONTEXT((#10995))
GLOBAL_UNIT_ASSIGNED_CONTEXT((#11036,#11038,#11039))
REPRESENTATION_CONTEXT('','3D')
);
#11029=(
GEOMETRIC_REPRESENTATION_CONTEXT(3)
GLOBAL_UNCERTAINTY_ASSIGNED_CONTEXT((#10996))
GLOBAL_UNIT_ASSIGNED_CONTEXT((#11036,#11038,#11039))
REPRESENTATION_CONTEXT('','3D')
);
#11030=(
GEOMETRIC_REPRESENTATION_CONTEXT(3)
GLOBAL_UNCERTAINTY_ASSIGNED_CONTEXT((#10997))
GLOBAL_UNIT_ASSIGNED_CONTEXT((#11036,#11038,#11039))
REPRESENTATION_CONTEXT('','3D')
);
#11031=(
GEOMETRIC_REPRESENTATION_CONTEXT(3)
GLOBAL_UNCERTAINTY_ASSIGNED_CONTEXT((#10998))
GLOBAL_UNIT_ASSIGNED_CONTEXT((#11036,#11038,#11039))
REPRESENTATION_CONTEXT('','3D')
);
#11032=(
GEOMETRIC_REPRESENTATION_CONTEXT(3)
GLOBAL_UNCERTAINTY_ASSIGNED_CONTEXT((#10999))
GLOBAL_UNIT_ASSIGNED_CONTEXT((#11036,#11038,#11039))
REPRESENTATION_CONTEXT('','3D')
);
#11033=(
GEOMETRIC_REPRESENTATION_CONTEXT(3)
GLOBAL_UNCERTAINTY_ASSIGNED_CONTEXT((#11000))
GLOBAL_UNIT_ASSIGNED_CONTEXT((#11036,#11038,#11039))
REPRESENTATION_CONTEXT('','3D')
);
#11034=(
GEOMETRIC_REPRESENTATION_CONTEXT(3)
GLOBAL_UNCERTAINTY_ASSIGNED_CONTEXT((#11001))
GLOBAL_UNIT_ASSIGNED_CONTEXT((#11036,#11038,#11039))
REPRESENTATION_CONTEXT('','3D')
);
#11035=(
GEOMETRIC_REPRESENTATION_CONTEXT(3)
GLOBAL_UNCERTAINTY_ASSIGNED_CONTEXT((#11002))
GLOBAL_UNIT_ASSIGNED_CONTEXT((#11036,#11038,#11039))
REPRESENTATION_CONTEXT('','3D')
);
#11036=(
LENGTH_UNIT()
NAMED_UNIT(*)
SI_UNIT(.CENTI.,.METRE.)
);
#11037=(
LENGTH_UNIT()
NAMED_UNIT(*)
SI_UNIT($,.METRE.)
);
#11038=(
NAMED_UNIT(*)
PLANE_ANGLE_UNIT()
SI_UNIT($,.RADIAN.)
);
#11039=(
NAMED_UNIT(*)
SI_UNIT($,.STERADIAN.)
SOLID_ANGLE_UNIT()
);
#11040=SHAPE_DEFINITION_REPRESENTATION(#11072,#11153);
#11041=SHAPE_DEFINITION_REPRESENTATION(#11073,#11154);
#11042=SHAPE_DEFINITION_REPRESENTATION(#11074,#11155);
#11043=SHAPE_DEFINITION_REPRESENTATION(#11075,#11156);
#11044=SHAPE_DEFINITION_REPRESENTATION(#11076,#11157);
#11045=SHAPE_DEFINITION_REPRESENTATION(#11077,#11158);
#11046=SHAPE_DEFINITION_REPRESENTATION(#11078,#11159);
#11047=SHAPE_DEFINITION_REPRESENTATION(#11079,#11160);
#11048=SHAPE_DEFINITION_REPRESENTATION(#11080,#11161);
#11049=SHAPE_DEFINITION_REPRESENTATION(#11081,#11162);
#11050=SHAPE_DEFINITION_REPRESENTATION(#11082,#11163);
#11051=SHAPE_DEFINITION_REPRESENTATION(#11083,#11164);
#11052=SHAPE_DEFINITION_REPRESENTATION(#11086,#11165);
#11053=SHAPE_DEFINITION_REPRESENTATION(#11087,#11166);
#11054=SHAPE_DEFINITION_REPRESENTATION(#11088,#11167);
#11055=SHAPE_DEFINITION_REPRESENTATION(#11089,#11168);
#11056=SHAPE_DEFINITION_REPRESENTATION(#11090,#11169);
#11057=SHAPE_DEFINITION_REPRESENTATION(#11091,#11170);
#11058=SHAPE_DEFINITION_REPRESENTATION(#11096,#11171);
#11059=SHAPE_DEFINITION_REPRESENTATION(#11097,#11172);
#11060=SHAPE_DEFINITION_REPRESENTATION(#11098,#11173);
#11061=SHAPE_DEFINITION_REPRESENTATION(#11099,#11174);
#11062=SHAPE_DEFINITION_REPRESENTATION(#11100,#11175);
#11063=SHAPE_DEFINITION_REPRESENTATION(#11101,#11176);
#11064=SHAPE_DEFINITION_REPRESENTATION(#11102,#11177);
#11065=SHAPE_DEFINITION_REPRESENTATION(#11109,#11178);
#11066=SHAPE_DEFINITION_REPRESENTATION(#11110,#11179);
#11067=SHAPE_DEFINITION_REPRESENTATION(#11111,#11180);
#11068=SHAPE_DEFINITION_REPRESENTATION(#11112,#11181);
#11069=SHAPE_DEFINITION_REPRESENTATION(#11113,#11182);
#11070=SHAPE_DEFINITION_REPRESENTATION(#11114,#11183);
#11071=SHAPE_DEFINITION_REPRESENTATION(#11115,#11184);
#11072=PRODUCT_DEFINITION_SHAPE('',$,#11186);
#11073=PRODUCT_DEFINITION_SHAPE('',$,#11187);
#11074=PRODUCT_DEFINITION_SHAPE('',$,#11188);
#11075=PRODUCT_DEFINITION_SHAPE('',$,#11189);
#11076=PRODUCT_DEFINITION_SHAPE('',$,#11190);
#11077=PRODUCT_DEFINITION_SHAPE('',$,#11191);
#11078=PRODUCT_DEFINITION_SHAPE('',$,#11192);
#11079=PRODUCT_DEFINITION_SHAPE('',$,#11193);
#11080=PRODUCT_DEFINITION_SHAPE('',$,#11194);
#11081=PRODUCT_DEFINITION_SHAPE('',$,#11195);
#11082=PRODUCT_DEFINITION_SHAPE('',$,#11196);
#11083=PRODUCT_DEFINITION_SHAPE('',$,#11197);
#11084=PRODUCT_DEFINITION_SHAPE($,$,#191);
#11085=PRODUCT_DEFINITION_SHAPE($,$,#192);
#11086=PRODUCT_DEFINITION_SHAPE('',$,#11198);
#11087=PRODUCT_DEFINITION_SHAPE('',$,#11199);
#11088=PRODUCT_DEFINITION_SHAPE('',$,#11200);
#11089=PRODUCT_DEFINITION_SHAPE('',$,#11201);
#11090=PRODUCT_DEFINITION_SHAPE('',$,#11202);
#11091=PRODUCT_DEFINITION_SHAPE('',$,#11203);
#11092=PRODUCT_DEFINITION_SHAPE($,$,#193);
#11093=PRODUCT_DEFINITION_SHAPE($,$,#194);
#11094=PRODUCT_DEFINITION_SHAPE($,$,#195);
#11095=PRODUCT_DEFINITION_SHAPE($,$,#196);
#11096=PRODUCT_DEFINITION_SHAPE('',$,#11204);
#11097=PRODUCT_DEFINITION_SHAPE('',$,#11205);
#11098=PRODUCT_DEFINITION_SHAPE('',$,#11206);
#11099=PRODUCT_DEFINITION_SHAPE('',$,#11207);
#11100=PRODUCT_DEFINITION_SHAPE('',$,#11208);
#11101=PRODUCT_DEFINITION_SHAPE('',$,#11209);
#11102=PRODUCT_DEFINITION_SHAPE('',$,#11210);
#11103=PRODUCT_DEFINITION_SHAPE($,$,#197);
#11104=PRODUCT_DEFINITION_SHAPE($,$,#198);
#11105=PRODUCT_DEFINITION_SHAPE($,$,#199);
#11106=PRODUCT_DEFINITION_SHAPE($,$,#200);
#11107=PRODUCT_DEFINITION_SHAPE($,$,#201);
#11108=PRODUCT_DEFINITION_SHAPE($,$,#202);
#11109=PRODUCT_DEFINITION_SHAPE('',$,#11211);
#11110=PRODUCT_DEFINITION_SHAPE('',$,#11212);
#11111=PRODUCT_DEFINITION_SHAPE('',$,#11213);
#11112=PRODUCT_DEFINITION_SHAPE('',$,#11214);
#11113=PRODUCT_DEFINITION_SHAPE('',$,#11215);
#11114=PRODUCT_DEFINITION_SHAPE('',$,#11216);
#11115=PRODUCT_DEFINITION_SHAPE('',$,#11217);
#11116=PRODUCT_DEFINITION_SHAPE($,$,#203);
#11117=PRODUCT_DEFINITION_SHAPE($,$,#204);
#11118=PRODUCT_DEFINITION_SHAPE($,$,#205);
#11119=PRODUCT_DEFINITION_SHAPE($,$,#206);
#11120=PRODUCT_DEFINITION_SHAPE($,$,#207);
#11121=PRODUCT_DEFINITION_SHAPE($,$,#208);
#11122=PRODUCT_DEFINITION_SHAPE($,$,#209);
#11123=PRODUCT_DEFINITION_SHAPE($,$,#210);
#11124=PRODUCT_DEFINITION_SHAPE($,$,#211);
#11125=PRODUCT_DEFINITION_SHAPE($,$,#212);
#11126=PRODUCT_DEFINITION_SHAPE($,$,#213);
#11127=PRODUCT_DEFINITION_SHAPE($,$,#214);
#11128=PRODUCT_DEFINITION_SHAPE($,$,#215);
#11129=PRODUCT_DEFINITION_SHAPE($,$,#216);
#11130=PRODUCT_DEFINITION_SHAPE($,$,#217);
#11131=PRODUCT_DEFINITION_SHAPE($,$,#218);
#11132=PRODUCT_DEFINITION_SHAPE($,$,#219);
#11133=PRODUCT_DEFINITION_SHAPE($,$,#220);
#11134=PRODUCT_DEFINITION_SHAPE($,$,#221);
#11135=PRODUCT_DEFINITION_SHAPE($,$,#222);
#11136=PRODUCT_DEFINITION_SHAPE($,$,#223);
#11137=PRODUCT_DEFINITION_SHAPE($,$,#224);
#11138=PRODUCT_DEFINITION_SHAPE($,$,#225);
#11139=PRODUCT_DEFINITION_SHAPE($,$,#226);
#11140=PRODUCT_DEFINITION_SHAPE($,$,#227);
#11141=PRODUCT_DEFINITION_SHAPE($,$,#228);
#11142=PRODUCT_DEFINITION_SHAPE($,$,#229);
#11143=PRODUCT_DEFINITION_SHAPE($,$,#230);
#11144=PRODUCT_DEFINITION_SHAPE($,$,#231);
#11145=PRODUCT_DEFINITION_SHAPE($,$,#232);
#11146=PRODUCT_DEFINITION_SHAPE($,$,#233);
#11147=PRODUCT_DEFINITION_SHAPE($,$,#234);
#11148=PRODUCT_DEFINITION_SHAPE($,$,#235);
#11149=PRODUCT_DEFINITION_SHAPE($,$,#236);
#11150=PRODUCT_DEFINITION_SHAPE($,$,#237);
#11151=PRODUCT_DEFINITION_SHAPE($,$,#238);
#11152=PRODUCT_DEFINITION_SHAPE($,$,#239);
#11153=SHAPE_REPRESENTATION('',(#5016,#5664,#5665,#5666,#5667),#11003);
#11154=SHAPE_REPRESENTATION('',(#5017,#5636,#5637,#5638,#5639,#5640,#5641,
#5642,#5643,#5644,#5645,#5646,#5647,#5648,#5649,#5650,#5651,#5652,#5653,
#5654,#5655,#5656,#5657,#5658,#5659,#5660,#5661,#5662),#11004);
#11155=SHAPE_REPRESENTATION('',(#5018),#11005);
#11156=SHAPE_REPRESENTATION('',(#5043),#11006);
#11157=SHAPE_REPRESENTATION('',(#5083),#11007);
#11158=SHAPE_REPRESENTATION('',(#5113),#11008);
#11159=SHAPE_REPRESENTATION('',(#5143),#11009);
#11160=SHAPE_REPRESENTATION('',(#5148),#11010);
#11161=SHAPE_REPRESENTATION('',(#5218),#11011);
#11162=SHAPE_REPRESENTATION('',(#5259,#5309,#5310),#11012);
#11163=SHAPE_REPRESENTATION('',(#5260),#11013);
#11164=SHAPE_REPRESENTATION('',(#5292),#11014);
#11165=SHAPE_REPRESENTATION('',(#5311),#11015);
#11166=SHAPE_REPRESENTATION('',(#5335,#5392,#5393,#5394,#5395),#11016);
#11167=SHAPE_REPRESENTATION('',(#5336),#11017);
#11168=SHAPE_REPRESENTATION('',(#5354),#11018);
#11169=SHAPE_REPRESENTATION('',(#5363),#11019);
#11170=SHAPE_REPRESENTATION('',(#5377),#11020);
#11171=SHAPE_REPRESENTATION('',(#5396,#5495,#5496,#5497,#5498,#5499,#5500),
#11021);
#11172=SHAPE_REPRESENTATION('',(#5397),#11022);
#11173=SHAPE_REPRESENTATION('',(#5430),#11023);
#11174=SHAPE_REPRESENTATION('',(#5444),#11024);
#11175=SHAPE_REPRESENTATION('',(#5453),#11025);
#11176=SHAPE_REPRESENTATION('',(#5462),#11026);
#11177=SHAPE_REPRESENTATION('',(#5471),#11027);
#11178=SHAPE_REPRESENTATION('',(#5501,#5663),#11028);
#11179=SHAPE_REPRESENTATION('',(#5502,#5631,#5632,#5633,#5634,#5635),#11029);
#11180=SHAPE_REPRESENTATION('',(#5503),#11030);
#11181=SHAPE_REPRESENTATION('',(#5523),#11031);
#11182=SHAPE_REPRESENTATION('',(#5543),#11032);
#11183=SHAPE_REPRESENTATION('',(#5560),#11033);
#11184=SHAPE_REPRESENTATION('',(#5614),#11034);
#11185=PRODUCT_DEFINITION_CONTEXT('part definition',#11283,'design');
#11186=PRODUCT_DEFINITION('PAT-099',
'PAT-099',#11218,#11185);
#11187=PRODUCT_DEFINITION('Base bearing and follower guide',
'Base bearing and follower guide',#11219,#11185);
#11188=PRODUCT_DEFINITION('Cam demonstrator base',
'Cam demonstrator base',#11220,#11185);
#11189=PRODUCT_DEFINITION('Linear follower guide',
'Linear follower guide',#11221,#11185);
#11190=PRODUCT_DEFINITION('Linear guide retaining cap',
'Linear guide retaining cap',#11222,#11185);
#11191=PRODUCT_DEFINITION('Linear guide retaining cap (1)',
'Linear guide retaining cap (1)',#11223,#11185);
#11192=PRODUCT_DEFINITION('Installed follower spring',
'Installed follower spring',#11224,#11185);
#11193=PRODUCT_DEFINITION('Pivot pedestal','Pivot pedestal',#11225,#11185);
#11194=PRODUCT_DEFINITION('Pivot cap','Pivot cap',#11226,#11185);
#11195=PRODUCT_DEFINITION('Linear Ball Bushing - 12 x 21 x 30 mm',
'Linear Ball Bushing - 12 x 21 x 30 mm',#11227,#11185);
#11196=PRODUCT_DEFINITION('Steel sleeve','Steel sleeve',#11228,#11185);
#11197=PRODUCT_DEFINITION('Ball retainer (plastic)',
'Ball retainer (plastic)',#11229,#11185);
#11198=PRODUCT_DEFINITION('M5x14 Cap Screw','M5x14 Cap Screw',#11230,#11185);
#11199=PRODUCT_DEFINITION('Eccentric cam spindle',
'Eccentric cam spindle',#11231,#11185);
#11200=PRODUCT_DEFINITION('Eccentric cam and spindle',
'Eccentric cam and spindle',#11232,#11185);
#11201=PRODUCT_DEFINITION('Lower race sleeve','Lower race sleeve',#11233,
#11185);
#11202=PRODUCT_DEFINITION('Spindle collar','Spindle collar',#11234,#11185);
#11203=PRODUCT_DEFINITION('M4x4 collar screw','M4x4 collar screw',#11235,
#11185);
#11204=PRODUCT_DEFINITION('Guided follower and pin',
'Guided follower and pin',#11236,#11185);
#11205=PRODUCT_DEFINITION('Forked roller follower',
'Forked roller follower',#11237,#11185);
#11206=PRODUCT_DEFINITION('Roller axle','Roller axle',#11238,#11185);
#11207=PRODUCT_DEFINITION('Roller inner-race spacer',
'Roller inner-race spacer',#11239,#11185);
#11208=PRODUCT_DEFINITION('Roller inner-race spacer (1)',
'Roller inner-race spacer (1)',#11240,#11185);
#11209=PRODUCT_DEFINITION('Roller axle keeper','Roller axle keeper',#11241,
#11185);
#11210=PRODUCT_DEFINITION('M4x10 Cap Screw','M4x10 Cap Screw',#11242,#11185);
#11211=PRODUCT_DEFINITION('Bearing roller','Bearing roller',#11243,#11185);
#11212=PRODUCT_DEFINITION('Sealed Ball Bearing - 10 x 30 x 9 mm',
'Sealed Ball Bearing - 10 x 30 x 9 mm',#11244,#11185);
#11213=PRODUCT_DEFINITION('Inner ring','Inner ring',#11245,#11185);
#11214=PRODUCT_DEFINITION('Outer ring','Outer ring',#11246,#11185);
#11215=PRODUCT_DEFINITION('Balls','Balls',#11247,#11185);
#11216=PRODUCT_DEFINITION('Cage','Cage',#11248,#11185);
#11217=PRODUCT_DEFINITION('Seals 2RS','Seals 2RS',#11249,#11185);
#11218=PRODUCT_DEFINITION_FORMATION('',$,#11285);
#11219=PRODUCT_DEFINITION_FORMATION('',$,#11286);
#11220=PRODUCT_DEFINITION_FORMATION('',$,#11287);
#11221=PRODUCT_DEFINITION_FORMATION('',$,#11288);
#11222=PRODUCT_DEFINITION_FORMATION('',$,#11289);
#11223=PRODUCT_DEFINITION_FORMATION('',$,#11290);
#11224=PRODUCT_DEFINITION_FORMATION('',$,#11291);
#11225=PRODUCT_DEFINITION_FORMATION('',$,#11292);
#11226=PRODUCT_DEFINITION_FORMATION('',$,#11293);
#11227=PRODUCT_DEFINITION_FORMATION('',$,#11294);
#11228=PRODUCT_DEFINITION_FORMATION('',$,#11295);
#11229=PRODUCT_DEFINITION_FORMATION('',$,#11296);
#11230=PRODUCT_DEFINITION_FORMATION('',$,#11297);
#11231=PRODUCT_DEFINITION_FORMATION('',$,#11298);
#11232=PRODUCT_DEFINITION_FORMATION('',$,#11299);
#11233=PRODUCT_DEFINITION_FORMATION('',$,#11300);
#11234=PRODUCT_DEFINITION_FORMATION('',$,#11301);
#11235=PRODUCT_DEFINITION_FORMATION('',$,#11302);
#11236=PRODUCT_DEFINITION_FORMATION('',$,#11303);
#11237=PRODUCT_DEFINITION_FORMATION('',$,#11304);
#11238=PRODUCT_DEFINITION_FORMATION('',$,#11305);
#11239=PRODUCT_DEFINITION_FORMATION('',$,#11306);
#11240=PRODUCT_DEFINITION_FORMATION('',$,#11307);
#11241=PRODUCT_DEFINITION_FORMATION('',$,#11308);
#11242=PRODUCT_DEFINITION_FORMATION('',$,#11309);
#11243=PRODUCT_DEFINITION_FORMATION('',$,#11310);
#11244=PRODUCT_DEFINITION_FORMATION('',$,#11311);
#11245=PRODUCT_DEFINITION_FORMATION('',$,#11312);
#11246=PRODUCT_DEFINITION_FORMATION('',$,#11313);
#11247=PRODUCT_DEFINITION_FORMATION('',$,#11314);
#11248=PRODUCT_DEFINITION_FORMATION('',$,#11315);
#11249=PRODUCT_DEFINITION_FORMATION('',$,#11316);
#11250=PRODUCT_RELATED_PRODUCT_CATEGORY(
'PAT-099','PAT-099',
(#11285));
#11251=PRODUCT_RELATED_PRODUCT_CATEGORY(
'Base bearing and follower guide','Base bearing and follower guide',(#11286));
#11252=PRODUCT_RELATED_PRODUCT_CATEGORY('Cam demonstrator base',
'Cam demonstrator base',(#11287));
#11253=PRODUCT_RELATED_PRODUCT_CATEGORY('Linear follower guide',
'Linear follower guide',(#11288));
#11254=PRODUCT_RELATED_PRODUCT_CATEGORY('Linear guide retaining cap',
'Linear guide retaining cap',(#11289));
#11255=PRODUCT_RELATED_PRODUCT_CATEGORY(
'Linear guide retaining cap (1)','Linear guide retaining cap (1)',(#11290));
#11256=PRODUCT_RELATED_PRODUCT_CATEGORY('Installed follower spring',
'Installed follower spring',(#11291));
#11257=PRODUCT_RELATED_PRODUCT_CATEGORY('Pivot pedestal',
'Pivot pedestal',(#11292));
#11258=PRODUCT_RELATED_PRODUCT_CATEGORY('Pivot cap','Pivot cap',(#11293));
#11259=PRODUCT_RELATED_PRODUCT_CATEGORY(
'Linear Ball Bushing - 12 x 21 x 30 mm',
'Linear Ball Bushing - 12 x 21 x 30 mm',(#11294));
#11260=PRODUCT_RELATED_PRODUCT_CATEGORY('Steel sleeve','Steel sleeve',(#11295));
#11261=PRODUCT_RELATED_PRODUCT_CATEGORY('Ball retainer (plastic)',
'Ball retainer (plastic)',(#11296));
#11262=PRODUCT_RELATED_PRODUCT_CATEGORY('M5x14 Cap Screw',
'M5x14 Cap Screw',(#11297));
#11263=PRODUCT_RELATED_PRODUCT_CATEGORY('Eccentric cam spindle',
'Eccentric cam spindle',(#11298));
#11264=PRODUCT_RELATED_PRODUCT_CATEGORY('Eccentric cam and spindle',
'Eccentric cam and spindle',(#11299));
#11265=PRODUCT_RELATED_PRODUCT_CATEGORY('Lower race sleeve',
'Lower race sleeve',(#11300));
#11266=PRODUCT_RELATED_PRODUCT_CATEGORY('Spindle collar',
'Spindle collar',(#11301));
#11267=PRODUCT_RELATED_PRODUCT_CATEGORY('M4x4 collar screw',
'M4x4 collar screw',(#11302));
#11268=PRODUCT_RELATED_PRODUCT_CATEGORY('Guided follower and pin',
'Guided follower and pin',(#11303));
#11269=PRODUCT_RELATED_PRODUCT_CATEGORY('Forked roller follower',
'Forked roller follower',(#11304));
#11270=PRODUCT_RELATED_PRODUCT_CATEGORY('Roller axle','Roller axle',(#11305));
#11271=PRODUCT_RELATED_PRODUCT_CATEGORY('Roller inner-race spacer',
'Roller inner-race spacer',(#11306));
#11272=PRODUCT_RELATED_PRODUCT_CATEGORY('Roller inner-race spacer (1)',
'Roller inner-race spacer (1)',(#11307));
#11273=PRODUCT_RELATED_PRODUCT_CATEGORY('Roller axle keeper',
'Roller axle keeper',(#11308));
#11274=PRODUCT_RELATED_PRODUCT_CATEGORY('M4x10 Cap Screw',
'M4x10 Cap Screw',(#11309));
#11275=PRODUCT_RELATED_PRODUCT_CATEGORY('Bearing roller',
'Bearing roller',(#11310));
#11276=PRODUCT_RELATED_PRODUCT_CATEGORY(
'Sealed Ball Bearing - 10 x 30 x 9 mm',
'Sealed Ball Bearing - 10 x 30 x 9 mm',(#11311));
#11277=PRODUCT_RELATED_PRODUCT_CATEGORY('Inner ring','Inner ring',(#11312));
#11278=PRODUCT_RELATED_PRODUCT_CATEGORY('Outer ring','Outer ring',(#11313));
#11279=PRODUCT_RELATED_PRODUCT_CATEGORY('Balls','Balls',(#11314));
#11280=PRODUCT_RELATED_PRODUCT_CATEGORY('Cage','Cage',(#11315));
#11281=PRODUCT_RELATED_PRODUCT_CATEGORY('Seals 2RS','Seals 2RS',(#11316));
#11282=APPLICATION_PROTOCOL_DEFINITION('international standard',
'automotive_design',2009,#11283);
#11283=APPLICATION_CONTEXT(
'Core Data for Automotive Mechanical Design Process');
#11284=PRODUCT_CONTEXT('part definition',#11283,'mechanical');
#11285=PRODUCT('PAT-099',
'PAT-099','PAT-099',
(#11284));
#11286=PRODUCT('Base bearing and follower guide',
'Base bearing and follower guide','Base bearing and follower guide',(#11284));
#11287=PRODUCT('Cam demonstrator base','Cam demonstrator base',
'Cam demonstrator base',(#11284));
#11288=PRODUCT('Linear follower guide','Linear follower guide',
'Linear follower guide',(#11284));
#11289=PRODUCT('Linear guide retaining cap',
'Linear guide retaining cap','Linear guide retaining cap',(#11284));
#11290=PRODUCT('Linear guide retaining cap (1)',
'Linear guide retaining cap (1)','Linear guide retaining cap (1)',(#11284));
#11291=PRODUCT('Installed follower spring','Installed follower spring',
'Installed follower spring',(#11284));
#11292=PRODUCT('Pivot pedestal','Pivot pedestal','Pivot pedestal',(#11284));
#11293=PRODUCT('Pivot cap','Pivot cap','Pivot cap',(#11284));
#11294=PRODUCT('Linear Ball Bushing - 12 x 21 x 30 mm',
'Linear Ball Bushing - 12 x 21 x 30 mm',
'Linear Ball Bushing - 12 x 21 x 30 mm',(#11284));
#11295=PRODUCT('Steel sleeve','Steel sleeve','Steel sleeve',(#11284));
#11296=PRODUCT('Ball retainer (plastic)','Ball retainer (plastic)',
'Ball retainer (plastic)',(#11284));
#11297=PRODUCT('M5x14 Cap Screw','M5x14 Cap Screw','M5x14 Cap Screw',(#11284));
#11298=PRODUCT('Eccentric cam spindle','Eccentric cam spindle',
'Eccentric cam spindle',(#11284));
#11299=PRODUCT('Eccentric cam and spindle','Eccentric cam and spindle',
'Eccentric cam and spindle',(#11284));
#11300=PRODUCT('Lower race sleeve','Lower race sleeve',
'Lower race sleeve',(#11284));
#11301=PRODUCT('Spindle collar','Spindle collar','Spindle collar',(#11284));
#11302=PRODUCT('M4x4 collar screw','M4x4 collar screw',
'M4x4 collar screw',(#11284));
#11303=PRODUCT('Guided follower and pin','Guided follower and pin',
'Guided follower and pin',(#11284));
#11304=PRODUCT('Forked roller follower','Forked roller follower',
'Forked roller follower',(#11284));
#11305=PRODUCT('Roller axle','Roller axle','Roller axle',(#11284));
#11306=PRODUCT('Roller inner-race spacer','Roller inner-race spacer',
'Roller inner-race spacer',(#11284));
#11307=PRODUCT('Roller inner-race spacer (1)',
'Roller inner-race spacer (1)','Roller inner-race spacer (1)',(#11284));
#11308=PRODUCT('Roller axle keeper','Roller axle keeper',
'Roller axle keeper',(#11284));
#11309=PRODUCT('M4x10 Cap Screw','M4x10 Cap Screw','M4x10 Cap Screw',(#11284));
#11310=PRODUCT('Bearing roller','Bearing roller','Bearing roller',(#11284));
#11311=PRODUCT('Sealed Ball Bearing - 10 x 30 x 9 mm',
'Sealed Ball Bearing - 10 x 30 x 9 mm',
'Sealed Ball Bearing - 10 x 30 x 9 mm',(#11284));
#11312=PRODUCT('Inner ring','Inner ring','Inner ring',(#11284));
#11313=PRODUCT('Outer ring','Outer ring','Outer ring',(#11284));
#11314=PRODUCT('Balls','Balls','Balls',(#11284));
#11315=PRODUCT('Cage','Cage','Cage',(#11284));
#11316=PRODUCT('Seals 2RS','Seals 2RS','Seals 2RS',(#11284));
#11317=PRESENTATION_STYLE_ASSIGNMENT((#11323));
#11318=PRESENTATION_STYLE_ASSIGNMENT((#11324));
#11319=PRESENTATION_STYLE_ASSIGNMENT((#11325));
#11320=PRESENTATION_STYLE_ASSIGNMENT((#11326));
#11321=PRESENTATION_STYLE_ASSIGNMENT((#11327));
#11322=PRESENTATION_STYLE_ASSIGNMENT((#11328));
#11323=SURFACE_STYLE_USAGE(.BOTH.,#11329);
#11324=SURFACE_STYLE_USAGE(.BOTH.,#11330);
#11325=SURFACE_STYLE_USAGE(.BOTH.,#11331);
#11326=SURFACE_STYLE_USAGE(.BOTH.,#11332);
#11327=SURFACE_STYLE_USAGE(.BOTH.,#11333);
#11328=SURFACE_STYLE_USAGE(.BOTH.,#11334);
#11329=SURFACE_SIDE_STYLE('',(#11335));
#11330=SURFACE_SIDE_STYLE('',(#11336));
#11331=SURFACE_SIDE_STYLE('',(#11337));
#11332=SURFACE_SIDE_STYLE('',(#11338));
#11333=SURFACE_SIDE_STYLE('',(#11339));
#11334=SURFACE_SIDE_STYLE('',(#11340));
#11335=SURFACE_STYLE_FILL_AREA(#11341);
#11336=SURFACE_STYLE_FILL_AREA(#11342);
#11337=SURFACE_STYLE_FILL_AREA(#11343);
#11338=SURFACE_STYLE_FILL_AREA(#11344);
#11339=SURFACE_STYLE_FILL_AREA(#11345);
#11340=SURFACE_STYLE_FILL_AREA(#11346);
#11341=FILL_AREA_STYLE('Steel - Satin',(#11347));
#11342=FILL_AREA_STYLE('CAD Library Painted - Deep blue',(#11348));
#11343=FILL_AREA_STYLE('CAD Library Painted - Engineering blue',(#11349));
#11344=FILL_AREA_STYLE('CAD Library Painted - Steel gray',(#11350));
#11345=FILL_AREA_STYLE('CAD Library Painted - Graphite',(#11351));
#11346=FILL_AREA_STYLE('CAD Library Painted - Off white',(#11352));
#11347=FILL_AREA_STYLE_COLOUR('Steel - Satin',#11353);
#11348=FILL_AREA_STYLE_COLOUR('CAD Library Painted - Deep blue',#11354);
#11349=FILL_AREA_STYLE_COLOUR('CAD Library Painted - Engineering blue',
#11355);
#11350=FILL_AREA_STYLE_COLOUR('CAD Library Painted - Steel gray',#11356);
#11351=FILL_AREA_STYLE_COLOUR('CAD Library Painted - Graphite',#11357);
#11352=FILL_AREA_STYLE_COLOUR('CAD Library Painted - Off white',#11358);
#11353=COLOUR_RGB('Steel - Satin',0.627450980392157,0.627450980392157,0.627450980392157);
#11354=COLOUR_RGB('CAD Library Painted - Deep blue',0.0784313725490196,
0.203921568627451,0.349019607843137);
#11355=COLOUR_RGB('CAD Library Painted - Engineering blue',0.12156862745098,
0.356862745098039,0.6);
#11356=COLOUR_RGB('CAD Library Painted - Steel gray',0.592156862745098,
0.631372549019608,0.67843137254902);
#11357=COLOUR_RGB('CAD Library Painted - Graphite',0.0980392156862745,0.109803921568627,
0.125490196078431);
#11358=COLOUR_RGB('CAD Library Painted - Off white',0.909803921568627,0.901960784313726,
0.858823529411765);
#11359=COLOUR_RGB('Dark Blue',0.08,0.2,0.34);
#11360=FILL_AREA_STYLE_COLOUR('',#11359);
#11361=FILL_AREA_STYLE('',(#11360));
#11362=SURFACE_STYLE_FILL_AREA(#11361);
#11363=SURFACE_SIDE_STYLE('',(#11362));
#11364=SURFACE_STYLE_USAGE(.BOTH.,#11363);
#11365=PRESENTATION_STYLE_ASSIGNMENT((#11364));
#11366=COLOUR_RGB('Light Blue',0.38,0.62,0.78);
#11367=FILL_AREA_STYLE_COLOUR('',#11366);
#11368=FILL_AREA_STYLE('',(#11367));
#11369=SURFACE_STYLE_FILL_AREA(#11368);
#11370=SURFACE_SIDE_STYLE('',(#11369));
#11371=SURFACE_STYLE_USAGE(.BOTH.,#11370);
#11372=PRESENTATION_STYLE_ASSIGNMENT((#11371));
#11373=COLOUR_RGB('Sky Blue',0.24,0.69,0.87);
#11374=FILL_AREA_STYLE_COLOUR('',#11373);
#11375=FILL_AREA_STYLE('',(#11374));
#11376=SURFACE_STYLE_FILL_AREA(#11375);
#11377=SURFACE_SIDE_STYLE('',(#11376));
#11378=SURFACE_STYLE_USAGE(.BOTH.,#11377);
#11379=PRESENTATION_STYLE_ASSIGNMENT((#11378));
#11380=COLOUR_RGB('Grey',0.48,0.52,0.57);
#11381=FILL_AREA_STYLE_COLOUR('',#11380);
#11382=FILL_AREA_STYLE('',(#11381));
#11383=SURFACE_STYLE_FILL_AREA(#11382);
#11384=SURFACE_SIDE_STYLE('',(#11383));
#11385=SURFACE_STYLE_USAGE(.BOTH.,#11384);
#11386=PRESENTATION_STYLE_ASSIGNMENT((#11385));
#11387=COLOUR_RGB('Black',0.12,0.14,0.17);
#11388=FILL_AREA_STYLE_COLOUR('',#11387);
#11389=FILL_AREA_STYLE('',(#11388));
#11390=SURFACE_STYLE_FILL_AREA(#11389);
#11391=SURFACE_SIDE_STYLE('',(#11390));
#11392=SURFACE_STYLE_USAGE(.BOTH.,#11391);
#11393=PRESENTATION_STYLE_ASSIGNMENT((#11392));
#11394=COLOUR_RGB('Off White',0.89,0.88,0.83);
#11395=FILL_AREA_STYLE_COLOUR('',#11394);
#11396=FILL_AREA_STYLE('',(#11395));
#11397=SURFACE_STYLE_FILL_AREA(#11396);
#11398=SURFACE_SIDE_STYLE('',(#11397));
#11399=SURFACE_STYLE_USAGE(.BOTH.,#11398);
#11400=PRESENTATION_STYLE_ASSIGNMENT((#11399));
ENDSEC;
END-ISO-10303-21;
